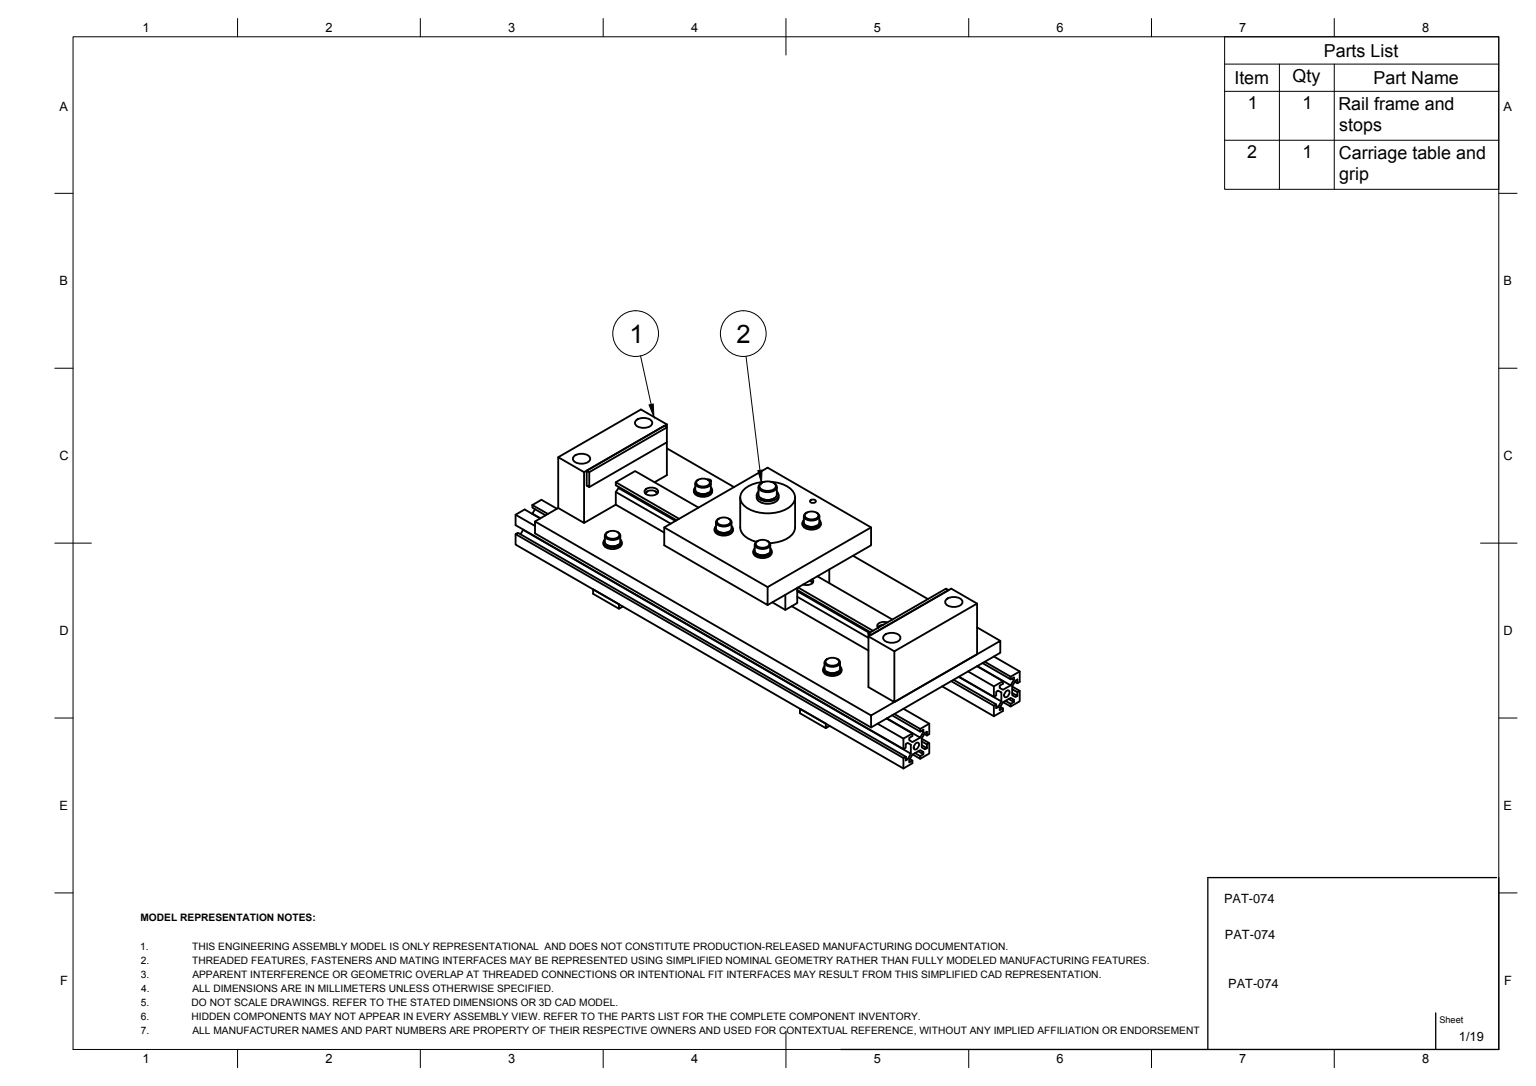
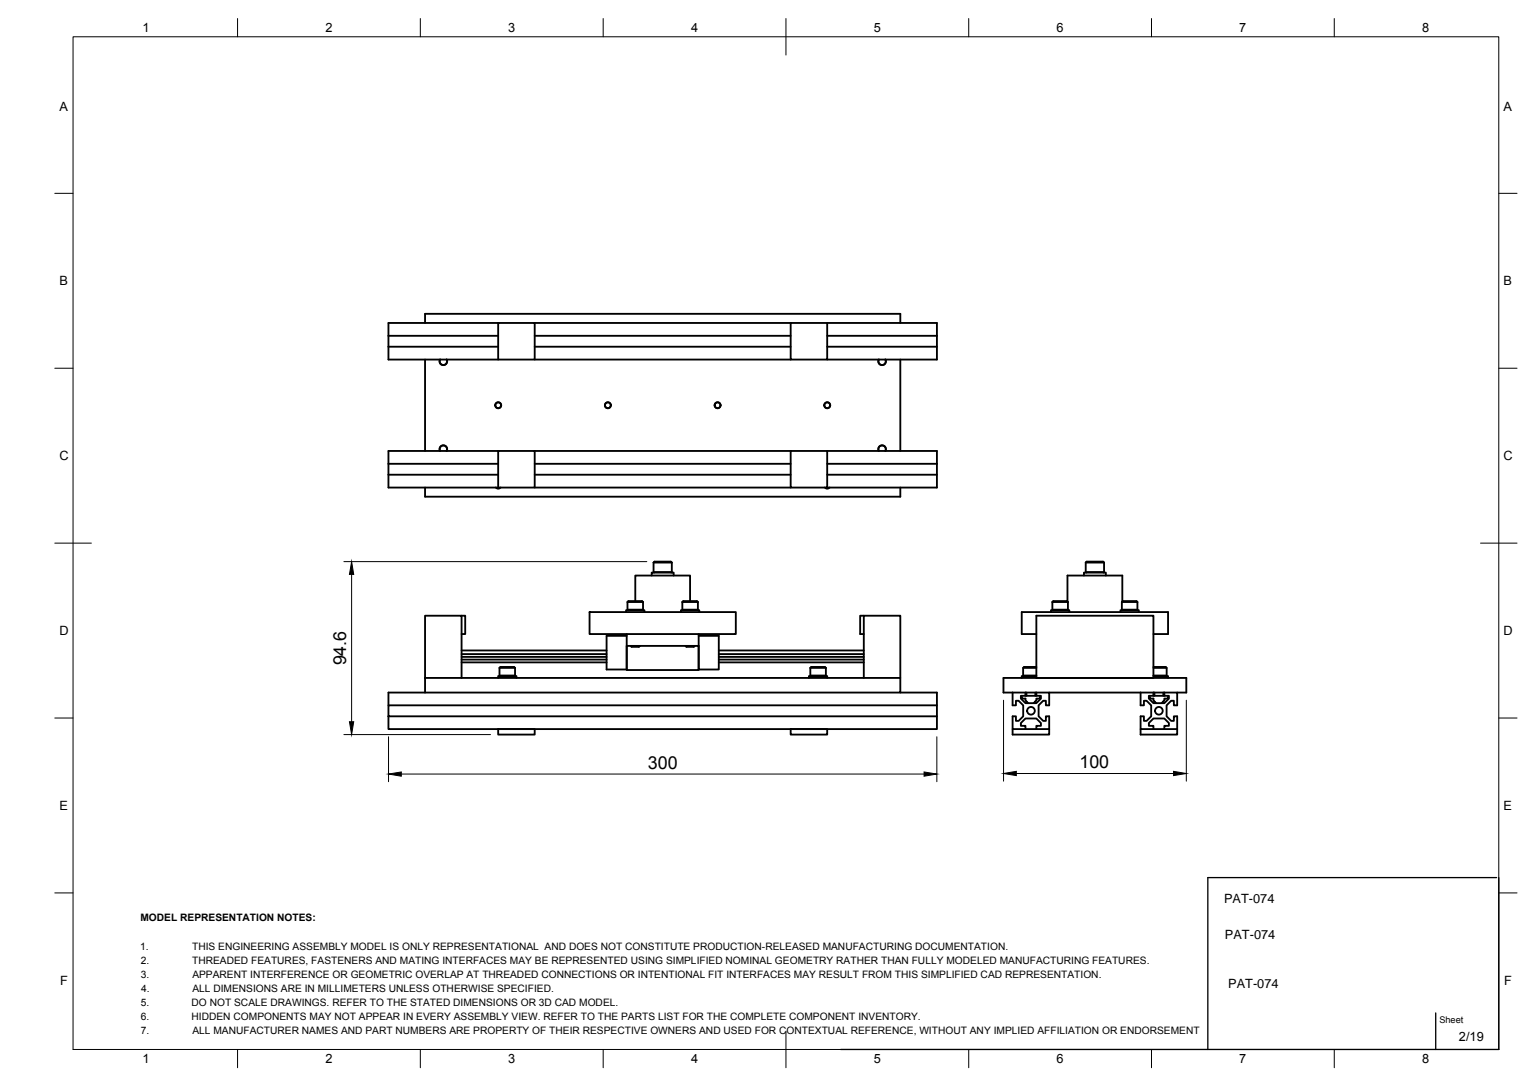
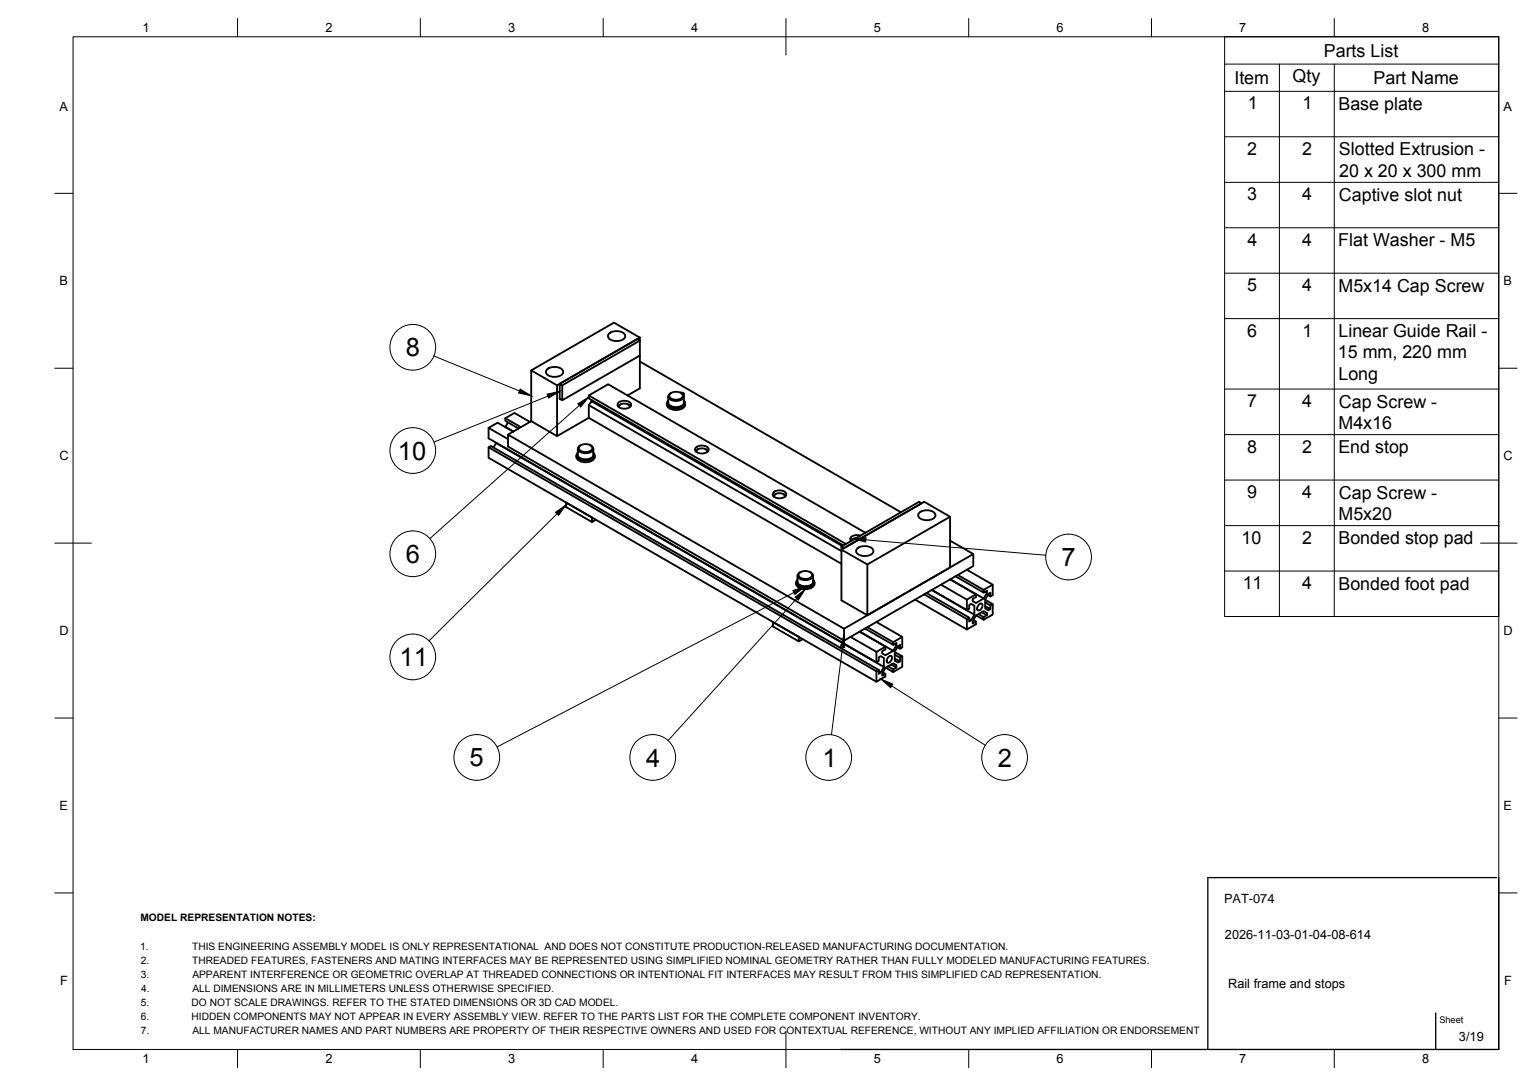
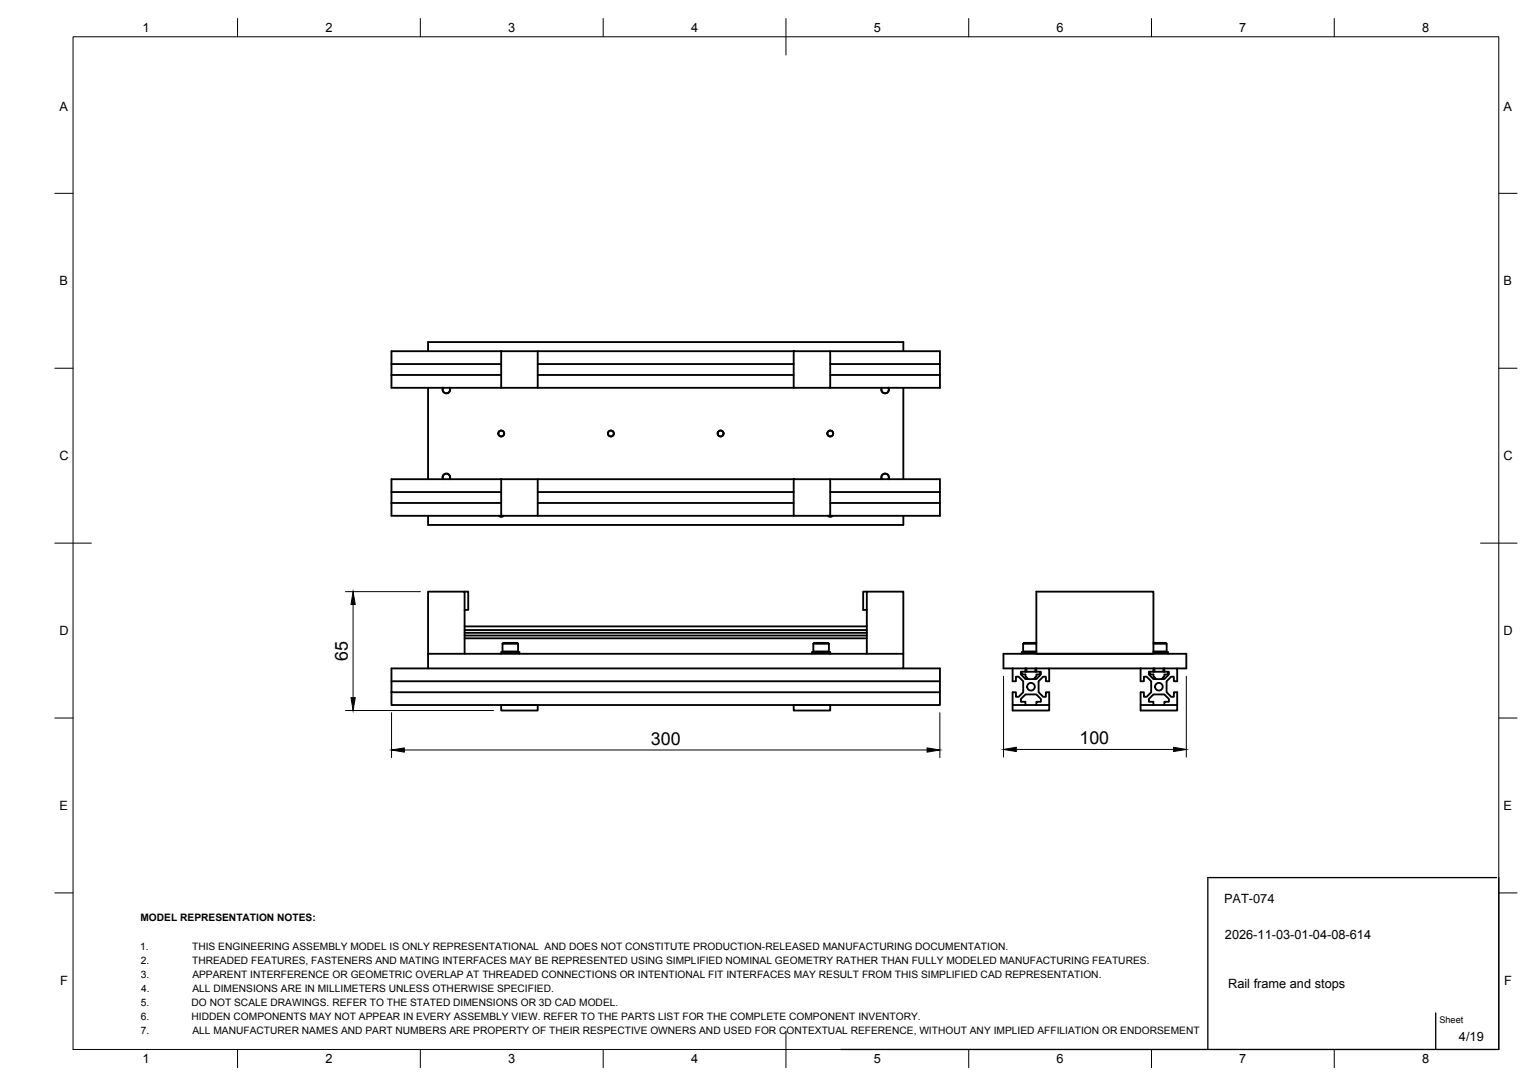
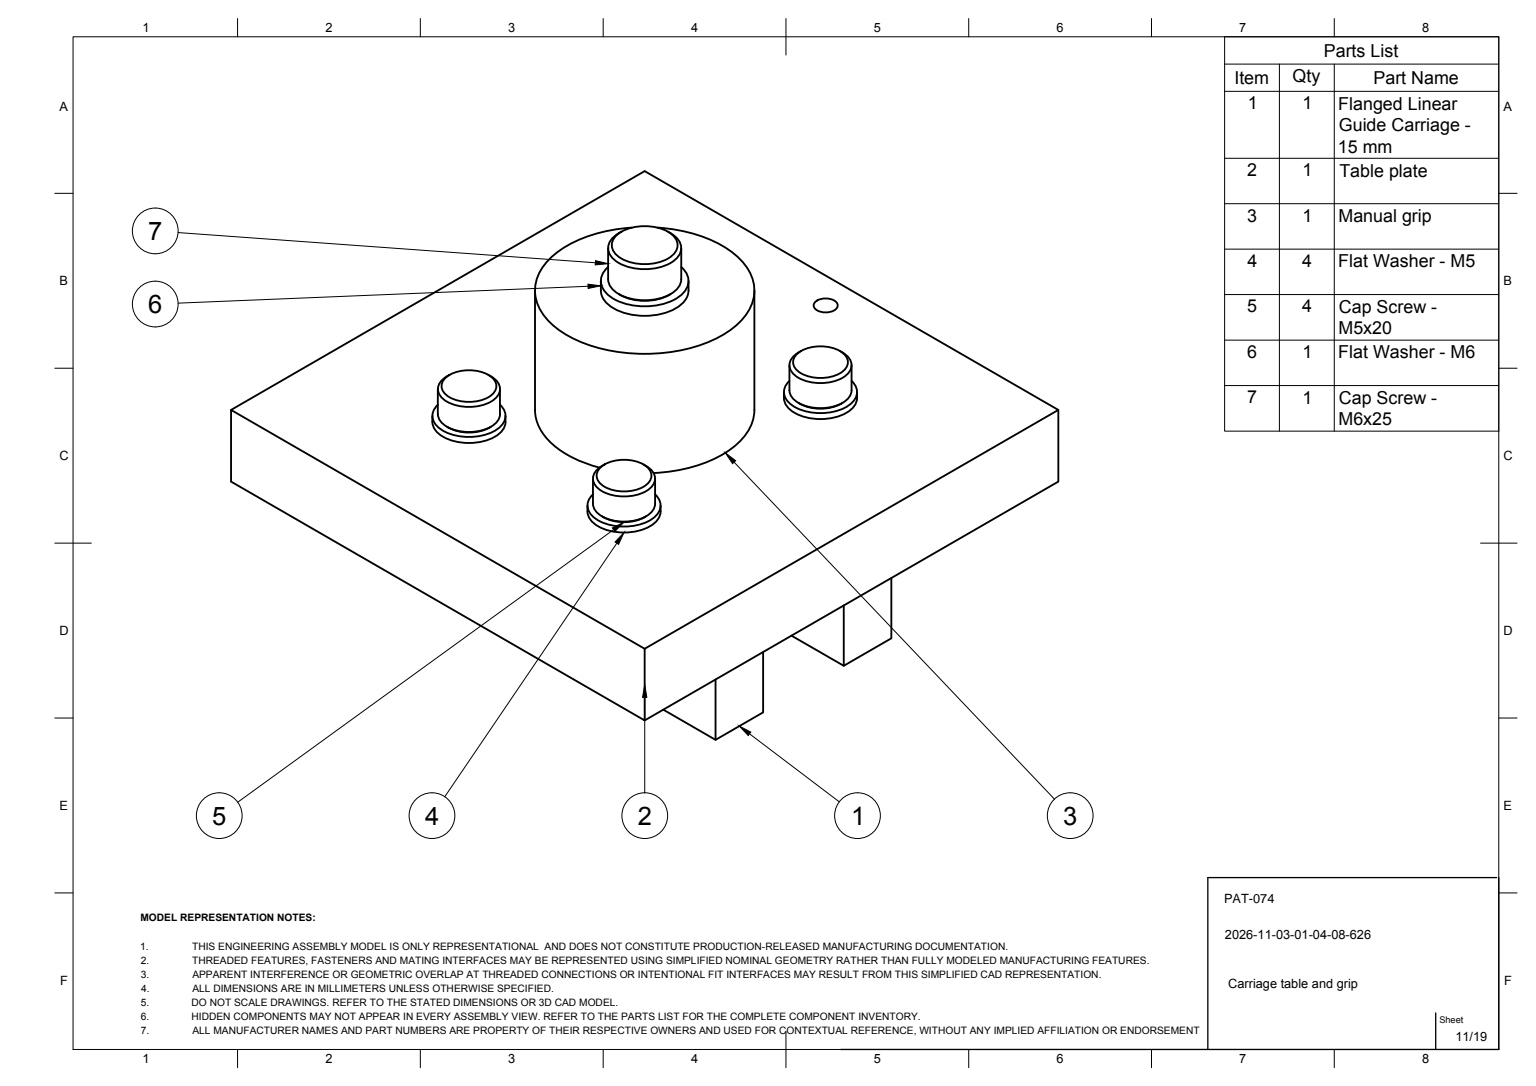
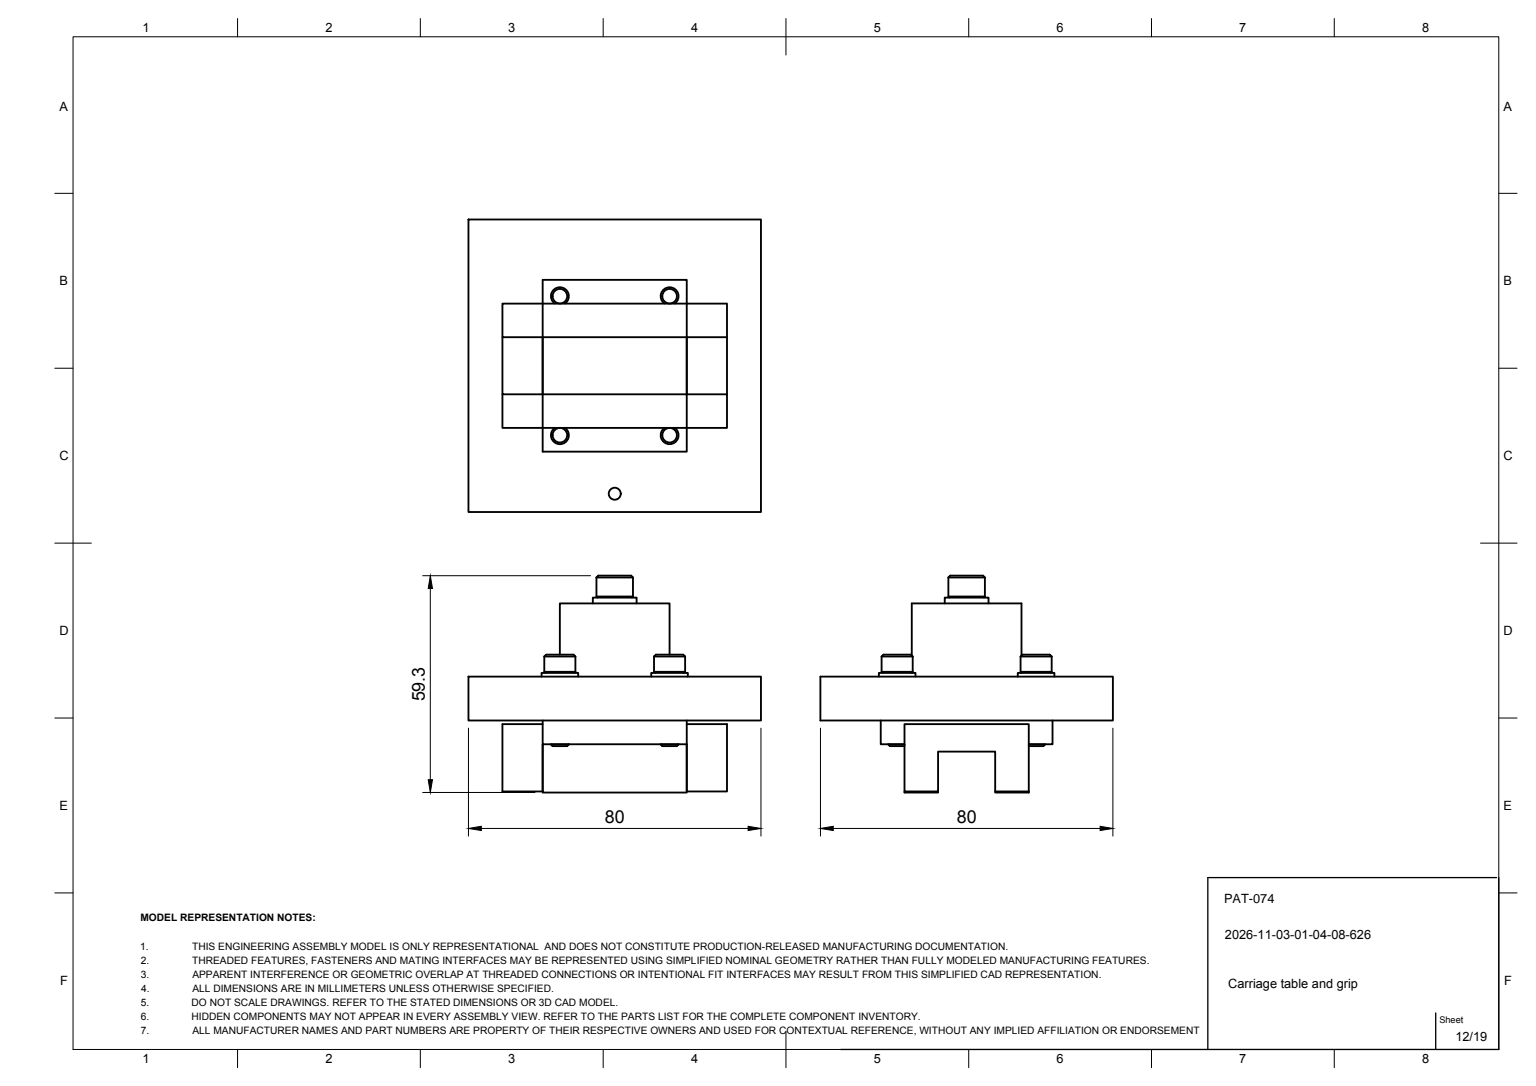
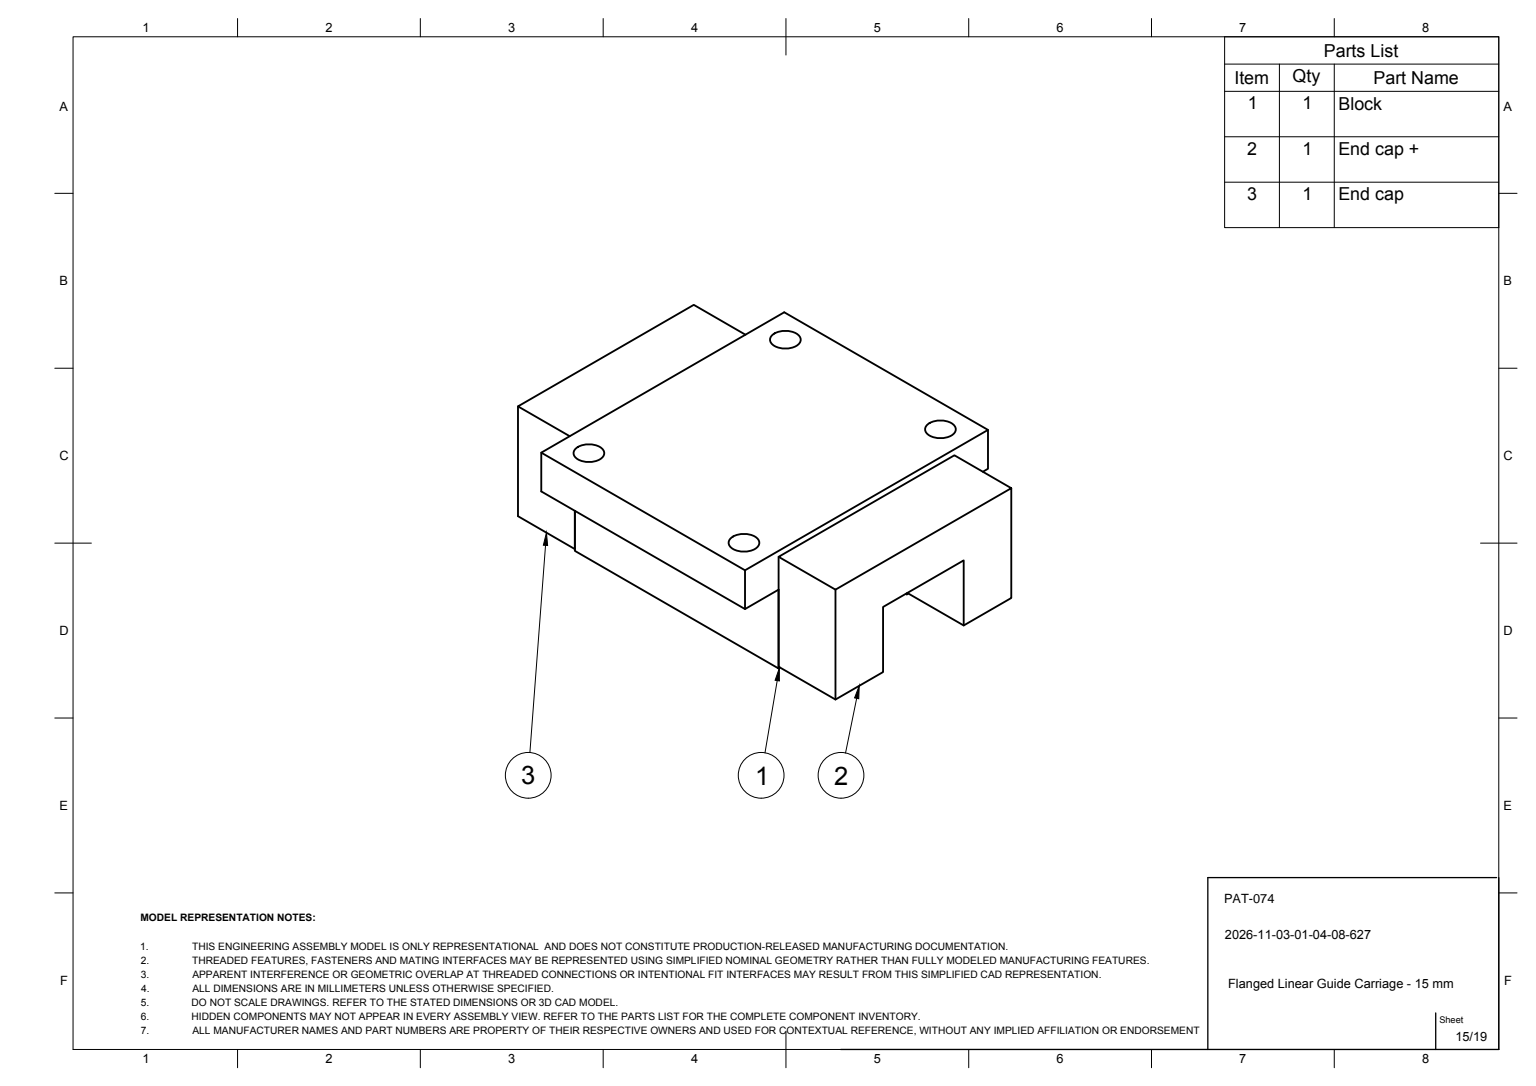
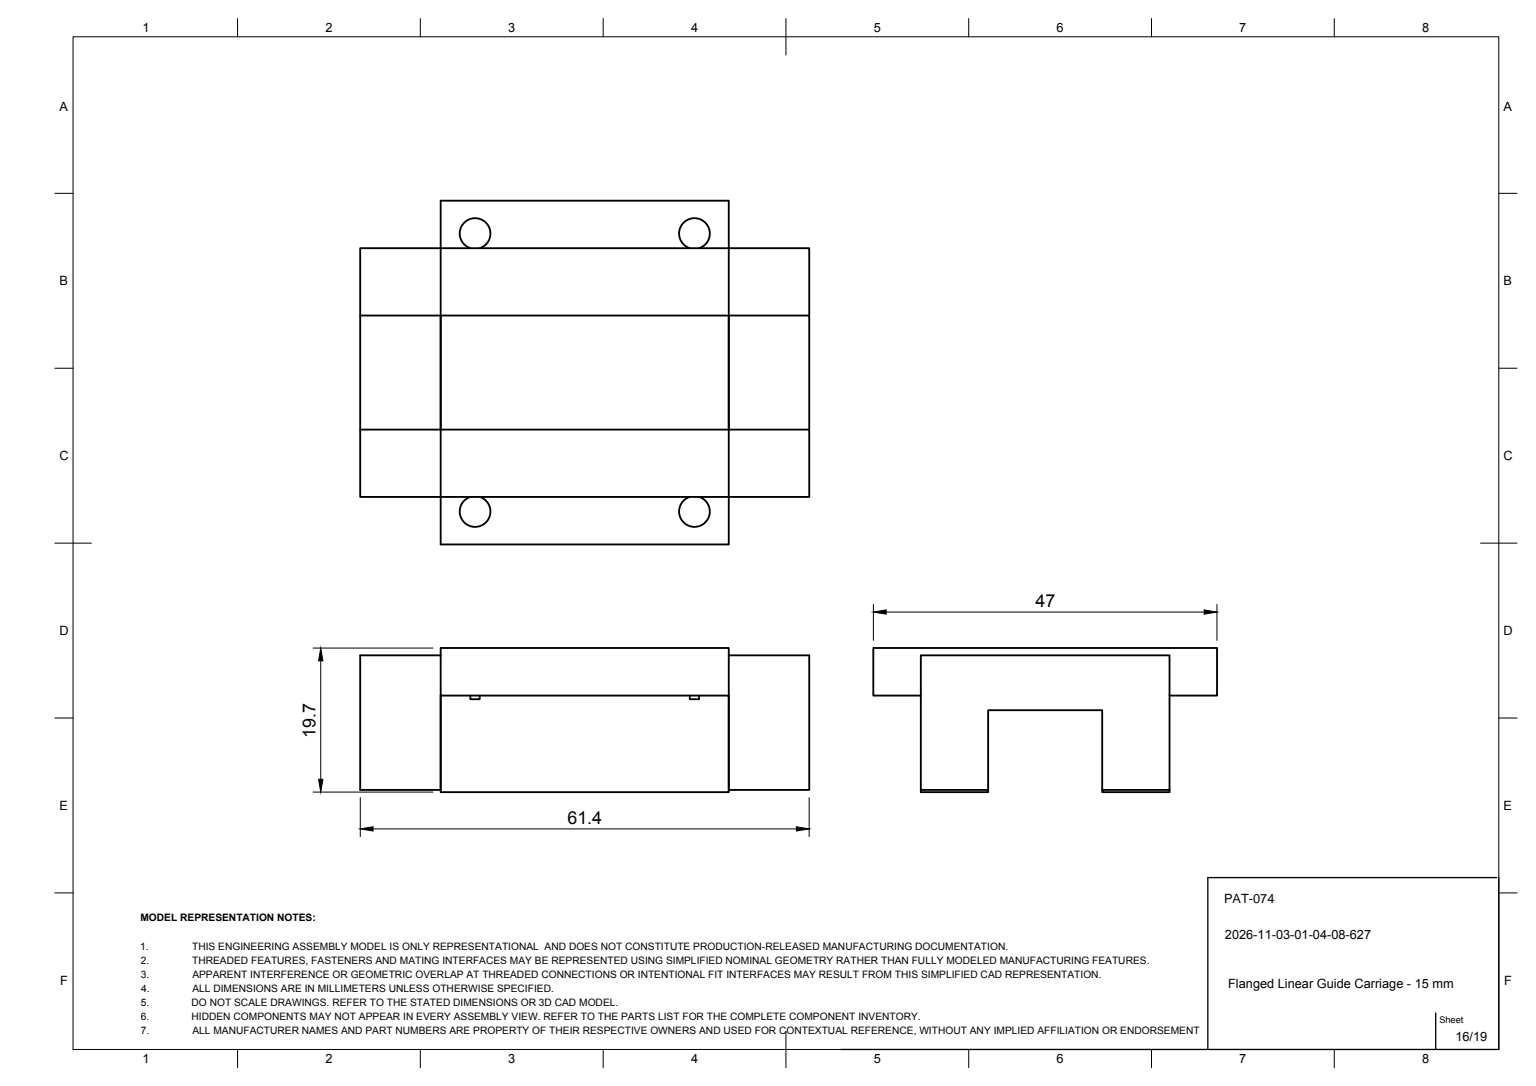
ISO-10303-21;
HEADER;
/* Generated by software containing ST-Developer
 * from STEP Tools, Inc. (www.steptools.com) 
 */

FILE_DESCRIPTION(
/* description */ ('Manual rail carriage with stops'),
/* implementation_level */ '2;1');

FILE_NAME(
/* name */ 'PAT-074',
/* time_stamp */ '2026-10-27T18:54:27-07:00',
/* author */ (''),
/* organization */ (''),
/* preprocessor_version */ 'ST-DEVELOPER v20.2',
/* originating_system */ 'Autodesk Translation Framework v15.17.0.0',
/* authorisation */ '');

FILE_SCHEMA (('AUTOMOTIVE_DESIGN { 1 0 10303 214 3 1 1 }'));
ENDSEC;

DATA;
#10=MECHANICAL_DESIGN_GEOMETRIC_PRESENTATION_REPRESENTATION('',(#273,#274,
#275,#276,#277,#278,#279,#280,#281,#282,#283,#284,#285,#286,#287,#288,#289,
#290),#8499);
#11=ITEM_DEFINED_TRANSFORMATION($,$,#5414,#5475);
#12=ITEM_DEFINED_TRANSFORMATION($,$,#5453,#5476);
#13=ITEM_DEFINED_TRANSFORMATION($,$,#5464,#5477);
#14=ITEM_DEFINED_TRANSFORMATION($,$,#5164,#5549);
#15=ITEM_DEFINED_TRANSFORMATION($,$,#5213,#5550);
#16=ITEM_DEFINED_TRANSFORMATION($,$,#5213,#5551);
#17=ITEM_DEFINED_TRANSFORMATION($,$,#5263,#5552);
#18=ITEM_DEFINED_TRANSFORMATION($,$,#5512,#5553);
#19=ITEM_DEFINED_TRANSFORMATION($,$,#5284,#5554);
#20=ITEM_DEFINED_TRANSFORMATION($,$,#5263,#5555);
#21=ITEM_DEFINED_TRANSFORMATION($,$,#5512,#5556);
#22=ITEM_DEFINED_TRANSFORMATION($,$,#5284,#5557);
#23=ITEM_DEFINED_TRANSFORMATION($,$,#5263,#5558);
#24=ITEM_DEFINED_TRANSFORMATION($,$,#5512,#5559);
#25=ITEM_DEFINED_TRANSFORMATION($,$,#5284,#5560);
#26=ITEM_DEFINED_TRANSFORMATION($,$,#5263,#5561);
#27=ITEM_DEFINED_TRANSFORMATION($,$,#5512,#5562);
#28=ITEM_DEFINED_TRANSFORMATION($,$,#5284,#5563);
#29=ITEM_DEFINED_TRANSFORMATION($,$,#5308,#5564);
#30=ITEM_DEFINED_TRANSFORMATION($,$,#5351,#5565);
#31=ITEM_DEFINED_TRANSFORMATION($,$,#5351,#5566);
#32=ITEM_DEFINED_TRANSFORMATION($,$,#5351,#5567);
#33=ITEM_DEFINED_TRANSFORMATION($,$,#5351,#5568);
#34=ITEM_DEFINED_TRANSFORMATION($,$,#5377,#5569);
#35=ITEM_DEFINED_TRANSFORMATION($,$,#5523,#5570);
#36=ITEM_DEFINED_TRANSFORMATION($,$,#5523,#5571);
#37=ITEM_DEFINED_TRANSFORMATION($,$,#5377,#5572);
#38=ITEM_DEFINED_TRANSFORMATION($,$,#5523,#5573);
#39=ITEM_DEFINED_TRANSFORMATION($,$,#5523,#5574);
#40=ITEM_DEFINED_TRANSFORMATION($,$,#5398,#5575);
#41=ITEM_DEFINED_TRANSFORMATION($,$,#5398,#5576);
#42=ITEM_DEFINED_TRANSFORMATION($,$,#5405,#5577);
#43=ITEM_DEFINED_TRANSFORMATION($,$,#5405,#5578);
#44=ITEM_DEFINED_TRANSFORMATION($,$,#5405,#5579);
#45=ITEM_DEFINED_TRANSFORMATION($,$,#5405,#5580);
#46=ITEM_DEFINED_TRANSFORMATION($,$,#5413,#5616);
#47=ITEM_DEFINED_TRANSFORMATION($,$,#5478,#5617);
#48=ITEM_DEFINED_TRANSFORMATION($,$,#5503,#5618);
#49=ITEM_DEFINED_TRANSFORMATION($,$,#5512,#5619);
#50=ITEM_DEFINED_TRANSFORMATION($,$,#5523,#5620);
#51=ITEM_DEFINED_TRANSFORMATION($,$,#5512,#5621);
#52=ITEM_DEFINED_TRANSFORMATION($,$,#5523,#5622);
#53=ITEM_DEFINED_TRANSFORMATION($,$,#5512,#5623);
#54=ITEM_DEFINED_TRANSFORMATION($,$,#5523,#5624);
#55=ITEM_DEFINED_TRANSFORMATION($,$,#5512,#5625);
#56=ITEM_DEFINED_TRANSFORMATION($,$,#5523,#5626);
#57=ITEM_DEFINED_TRANSFORMATION($,$,#5581,#5627);
#58=ITEM_DEFINED_TRANSFORMATION($,$,#5590,#5628);
#59=ITEM_DEFINED_TRANSFORMATION($,$,#5163,#5629);
#60=ITEM_DEFINED_TRANSFORMATION($,$,#5412,#5630);
#61=(
REPRESENTATION_RELATIONSHIP($,$,#8611,#8610)
REPRESENTATION_RELATIONSHIP_WITH_TRANSFORMATION(#11)
SHAPE_REPRESENTATION_RELATIONSHIP()
);
#62=(
REPRESENTATION_RELATIONSHIP($,$,#8612,#8610)
REPRESENTATION_RELATIONSHIP_WITH_TRANSFORMATION(#12)
SHAPE_REPRESENTATION_RELATIONSHIP()
);
#63=(
REPRESENTATION_RELATIONSHIP($,$,#8613,#8610)
REPRESENTATION_RELATIONSHIP_WITH_TRANSFORMATION(#13)
SHAPE_REPRESENTATION_RELATIONSHIP()
);
#64=(
REPRESENTATION_RELATIONSHIP($,$,#8600,#8599)
REPRESENTATION_RELATIONSHIP_WITH_TRANSFORMATION(#14)
SHAPE_REPRESENTATION_RELATIONSHIP()
);
#65=(
REPRESENTATION_RELATIONSHIP($,$,#8601,#8599)
REPRESENTATION_RELATIONSHIP_WITH_TRANSFORMATION(#15)
SHAPE_REPRESENTATION_RELATIONSHIP()
);
#66=(
REPRESENTATION_RELATIONSHIP($,$,#8601,#8599)
REPRESENTATION_RELATIONSHIP_WITH_TRANSFORMATION(#16)
SHAPE_REPRESENTATION_RELATIONSHIP()
);
#67=(
REPRESENTATION_RELATIONSHIP($,$,#8602,#8599)
REPRESENTATION_RELATIONSHIP_WITH_TRANSFORMATION(#17)
SHAPE_REPRESENTATION_RELATIONSHIP()
);
#68=(
REPRESENTATION_RELATIONSHIP($,$,#8616,#8599)
REPRESENTATION_RELATIONSHIP_WITH_TRANSFORMATION(#18)
SHAPE_REPRESENTATION_RELATIONSHIP()
);
#69=(
REPRESENTATION_RELATIONSHIP($,$,#8603,#8599)
REPRESENTATION_RELATIONSHIP_WITH_TRANSFORMATION(#19)
SHAPE_REPRESENTATION_RELATIONSHIP()
);
#70=(
REPRESENTATION_RELATIONSHIP($,$,#8602,#8599)
REPRESENTATION_RELATIONSHIP_WITH_TRANSFORMATION(#20)
SHAPE_REPRESENTATION_RELATIONSHIP()
);
#71=(
REPRESENTATION_RELATIONSHIP($,$,#8616,#8599)
REPRESENTATION_RELATIONSHIP_WITH_TRANSFORMATION(#21)
SHAPE_REPRESENTATION_RELATIONSHIP()
);
#72=(
REPRESENTATION_RELATIONSHIP($,$,#8603,#8599)
REPRESENTATION_RELATIONSHIP_WITH_TRANSFORMATION(#22)
SHAPE_REPRESENTATION_RELATIONSHIP()
);
#73=(
REPRESENTATION_RELATIONSHIP($,$,#8602,#8599)
REPRESENTATION_RELATIONSHIP_WITH_TRANSFORMATION(#23)
SHAPE_REPRESENTATION_RELATIONSHIP()
);
#74=(
REPRESENTATION_RELATIONSHIP($,$,#8616,#8599)
REPRESENTATION_RELATIONSHIP_WITH_TRANSFORMATION(#24)
SHAPE_REPRESENTATION_RELATIONSHIP()
);
#75=(
REPRESENTATION_RELATIONSHIP($,$,#8603,#8599)
REPRESENTATION_RELATIONSHIP_WITH_TRANSFORMATION(#25)
SHAPE_REPRESENTATION_RELATIONSHIP()
);
#76=(
REPRESENTATION_RELATIONSHIP($,$,#8602,#8599)
REPRESENTATION_RELATIONSHIP_WITH_TRANSFORMATION(#26)
SHAPE_REPRESENTATION_RELATIONSHIP()
);
#77=(
REPRESENTATION_RELATIONSHIP($,$,#8616,#8599)
REPRESENTATION_RELATIONSHIP_WITH_TRANSFORMATION(#27)
SHAPE_REPRESENTATION_RELATIONSHIP()
);
#78=(
REPRESENTATION_RELATIONSHIP($,$,#8603,#8599)
REPRESENTATION_RELATIONSHIP_WITH_TRANSFORMATION(#28)
SHAPE_REPRESENTATION_RELATIONSHIP()
);
#79=(
REPRESENTATION_RELATIONSHIP($,$,#8604,#8599)
REPRESENTATION_RELATIONSHIP_WITH_TRANSFORMATION(#29)
SHAPE_REPRESENTATION_RELATIONSHIP()
);
#80=(
REPRESENTATION_RELATIONSHIP($,$,#8605,#8599)
REPRESENTATION_RELATIONSHIP_WITH_TRANSFORMATION(#30)
SHAPE_REPRESENTATION_RELATIONSHIP()
);
#81=(
REPRESENTATION_RELATIONSHIP($,$,#8605,#8599)
REPRESENTATION_RELATIONSHIP_WITH_TRANSFORMATION(#31)
SHAPE_REPRESENTATION_RELATIONSHIP()
);
#82=(
REPRESENTATION_RELATIONSHIP($,$,#8605,#8599)
REPRESENTATION_RELATIONSHIP_WITH_TRANSFORMATION(#32)
SHAPE_REPRESENTATION_RELATIONSHIP()
);
#83=(
REPRESENTATION_RELATIONSHIP($,$,#8605,#8599)
REPRESENTATION_RELATIONSHIP_WITH_TRANSFORMATION(#33)
SHAPE_REPRESENTATION_RELATIONSHIP()
);
#84=(
REPRESENTATION_RELATIONSHIP($,$,#8606,#8599)
REPRESENTATION_RELATIONSHIP_WITH_TRANSFORMATION(#34)
SHAPE_REPRESENTATION_RELATIONSHIP()
);
#85=(
REPRESENTATION_RELATIONSHIP($,$,#8617,#8599)
REPRESENTATION_RELATIONSHIP_WITH_TRANSFORMATION(#35)
SHAPE_REPRESENTATION_RELATIONSHIP()
);
#86=(
REPRESENTATION_RELATIONSHIP($,$,#8617,#8599)
REPRESENTATION_RELATIONSHIP_WITH_TRANSFORMATION(#36)
SHAPE_REPRESENTATION_RELATIONSHIP()
);
#87=(
REPRESENTATION_RELATIONSHIP($,$,#8606,#8599)
REPRESENTATION_RELATIONSHIP_WITH_TRANSFORMATION(#37)
SHAPE_REPRESENTATION_RELATIONSHIP()
);
#88=(
REPRESENTATION_RELATIONSHIP($,$,#8617,#8599)
REPRESENTATION_RELATIONSHIP_WITH_TRANSFORMATION(#38)
SHAPE_REPRESENTATION_RELATIONSHIP()
);
#89=(
REPRESENTATION_RELATIONSHIP($,$,#8617,#8599)
REPRESENTATION_RELATIONSHIP_WITH_TRANSFORMATION(#39)
SHAPE_REPRESENTATION_RELATIONSHIP()
);
#90=(
REPRESENTATION_RELATIONSHIP($,$,#8607,#8599)
REPRESENTATION_RELATIONSHIP_WITH_TRANSFORMATION(#40)
SHAPE_REPRESENTATION_RELATIONSHIP()
);
#91=(
REPRESENTATION_RELATIONSHIP($,$,#8607,#8599)
REPRESENTATION_RELATIONSHIP_WITH_TRANSFORMATION(#41)
SHAPE_REPRESENTATION_RELATIONSHIP()
);
#92=(
REPRESENTATION_RELATIONSHIP($,$,#8608,#8599)
REPRESENTATION_RELATIONSHIP_WITH_TRANSFORMATION(#42)
SHAPE_REPRESENTATION_RELATIONSHIP()
);
#93=(
REPRESENTATION_RELATIONSHIP($,$,#8608,#8599)
REPRESENTATION_RELATIONSHIP_WITH_TRANSFORMATION(#43)
SHAPE_REPRESENTATION_RELATIONSHIP()
);
#94=(
REPRESENTATION_RELATIONSHIP($,$,#8608,#8599)
REPRESENTATION_RELATIONSHIP_WITH_TRANSFORMATION(#44)
SHAPE_REPRESENTATION_RELATIONSHIP()
);
#95=(
REPRESENTATION_RELATIONSHIP($,$,#8608,#8599)
REPRESENTATION_RELATIONSHIP_WITH_TRANSFORMATION(#45)
SHAPE_REPRESENTATION_RELATIONSHIP()
);
#96=(
REPRESENTATION_RELATIONSHIP($,$,#8610,#8609)
REPRESENTATION_RELATIONSHIP_WITH_TRANSFORMATION(#46)
SHAPE_REPRESENTATION_RELATIONSHIP()
);
#97=(
REPRESENTATION_RELATIONSHIP($,$,#8614,#8609)
REPRESENTATION_RELATIONSHIP_WITH_TRANSFORMATION(#47)
SHAPE_REPRESENTATION_RELATIONSHIP()
);
#98=(
REPRESENTATION_RELATIONSHIP($,$,#8615,#8609)
REPRESENTATION_RELATIONSHIP_WITH_TRANSFORMATION(#48)
SHAPE_REPRESENTATION_RELATIONSHIP()
);
#99=(
REPRESENTATION_RELATIONSHIP($,$,#8616,#8609)
REPRESENTATION_RELATIONSHIP_WITH_TRANSFORMATION(#49)
SHAPE_REPRESENTATION_RELATIONSHIP()
);
#100=(
REPRESENTATION_RELATIONSHIP($,$,#8617,#8609)
REPRESENTATION_RELATIONSHIP_WITH_TRANSFORMATION(#50)
SHAPE_REPRESENTATION_RELATIONSHIP()
);
#101=(
REPRESENTATION_RELATIONSHIP($,$,#8616,#8609)
REPRESENTATION_RELATIONSHIP_WITH_TRANSFORMATION(#51)
SHAPE_REPRESENTATION_RELATIONSHIP()
);
#102=(
REPRESENTATION_RELATIONSHIP($,$,#8617,#8609)
REPRESENTATION_RELATIONSHIP_WITH_TRANSFORMATION(#52)
SHAPE_REPRESENTATION_RELATIONSHIP()
);
#103=(
REPRESENTATION_RELATIONSHIP($,$,#8616,#8609)
REPRESENTATION_RELATIONSHIP_WITH_TRANSFORMATION(#53)
SHAPE_REPRESENTATION_RELATIONSHIP()
);
#104=(
REPRESENTATION_RELATIONSHIP($,$,#8617,#8609)
REPRESENTATION_RELATIONSHIP_WITH_TRANSFORMATION(#54)
SHAPE_REPRESENTATION_RELATIONSHIP()
);
#105=(
REPRESENTATION_RELATIONSHIP($,$,#8616,#8609)
REPRESENTATION_RELATIONSHIP_WITH_TRANSFORMATION(#55)
SHAPE_REPRESENTATION_RELATIONSHIP()
);
#106=(
REPRESENTATION_RELATIONSHIP($,$,#8617,#8609)
REPRESENTATION_RELATIONSHIP_WITH_TRANSFORMATION(#56)
SHAPE_REPRESENTATION_RELATIONSHIP()
);
#107=(
REPRESENTATION_RELATIONSHIP($,$,#8618,#8609)
REPRESENTATION_RELATIONSHIP_WITH_TRANSFORMATION(#57)
SHAPE_REPRESENTATION_RELATIONSHIP()
);
#108=(
REPRESENTATION_RELATIONSHIP($,$,#8619,#8609)
REPRESENTATION_RELATIONSHIP_WITH_TRANSFORMATION(#58)
SHAPE_REPRESENTATION_RELATIONSHIP()
);
#109=(
REPRESENTATION_RELATIONSHIP($,$,#8599,#8598)
REPRESENTATION_RELATIONSHIP_WITH_TRANSFORMATION(#59)
SHAPE_REPRESENTATION_RELATIONSHIP()
);
#110=(
REPRESENTATION_RELATIONSHIP($,$,#8609,#8598)
REPRESENTATION_RELATIONSHIP_WITH_TRANSFORMATION(#60)
SHAPE_REPRESENTATION_RELATIONSHIP()
);
#111=CONTEXT_DEPENDENT_SHAPE_REPRESENTATION(#61,#8542);
#112=CONTEXT_DEPENDENT_SHAPE_REPRESENTATION(#62,#8543);
#113=CONTEXT_DEPENDENT_SHAPE_REPRESENTATION(#63,#8544);
#114=CONTEXT_DEPENDENT_SHAPE_REPRESENTATION(#64,#8549);
#115=CONTEXT_DEPENDENT_SHAPE_REPRESENTATION(#65,#8550);
#116=CONTEXT_DEPENDENT_SHAPE_REPRESENTATION(#66,#8551);
#117=CONTEXT_DEPENDENT_SHAPE_REPRESENTATION(#67,#8552);
#118=CONTEXT_DEPENDENT_SHAPE_REPRESENTATION(#68,#8553);
#119=CONTEXT_DEPENDENT_SHAPE_REPRESENTATION(#69,#8554);
#120=CONTEXT_DEPENDENT_SHAPE_REPRESENTATION(#70,#8555);
#121=CONTEXT_DEPENDENT_SHAPE_REPRESENTATION(#71,#8556);
#122=CONTEXT_DEPENDENT_SHAPE_REPRESENTATION(#72,#8557);
#123=CONTEXT_DEPENDENT_SHAPE_REPRESENTATION(#73,#8558);
#124=CONTEXT_DEPENDENT_SHAPE_REPRESENTATION(#74,#8559);
#125=CONTEXT_DEPENDENT_SHAPE_REPRESENTATION(#75,#8560);
#126=CONTEXT_DEPENDENT_SHAPE_REPRESENTATION(#76,#8561);
#127=CONTEXT_DEPENDENT_SHAPE_REPRESENTATION(#77,#8562);
#128=CONTEXT_DEPENDENT_SHAPE_REPRESENTATION(#78,#8563);
#129=CONTEXT_DEPENDENT_SHAPE_REPRESENTATION(#79,#8564);
#130=CONTEXT_DEPENDENT_SHAPE_REPRESENTATION(#80,#8565);
#131=CONTEXT_DEPENDENT_SHAPE_REPRESENTATION(#81,#8566);
#132=CONTEXT_DEPENDENT_SHAPE_REPRESENTATION(#82,#8567);
#133=CONTEXT_DEPENDENT_SHAPE_REPRESENTATION(#83,#8568);
#134=CONTEXT_DEPENDENT_SHAPE_REPRESENTATION(#84,#8569);
#135=CONTEXT_DEPENDENT_SHAPE_REPRESENTATION(#85,#8570);
#136=CONTEXT_DEPENDENT_SHAPE_REPRESENTATION(#86,#8571);
#137=CONTEXT_DEPENDENT_SHAPE_REPRESENTATION(#87,#8572);
#138=CONTEXT_DEPENDENT_SHAPE_REPRESENTATION(#88,#8573);
#139=CONTEXT_DEPENDENT_SHAPE_REPRESENTATION(#89,#8574);
#140=CONTEXT_DEPENDENT_SHAPE_REPRESENTATION(#90,#8575);
#141=CONTEXT_DEPENDENT_SHAPE_REPRESENTATION(#91,#8576);
#142=CONTEXT_DEPENDENT_SHAPE_REPRESENTATION(#92,#8577);
#143=CONTEXT_DEPENDENT_SHAPE_REPRESENTATION(#93,#8578);
#144=CONTEXT_DEPENDENT_SHAPE_REPRESENTATION(#94,#8579);
#145=CONTEXT_DEPENDENT_SHAPE_REPRESENTATION(#95,#8580);
#146=CONTEXT_DEPENDENT_SHAPE_REPRESENTATION(#96,#8583);
#147=CONTEXT_DEPENDENT_SHAPE_REPRESENTATION(#97,#8584);
#148=CONTEXT_DEPENDENT_SHAPE_REPRESENTATION(#98,#8585);
#149=CONTEXT_DEPENDENT_SHAPE_REPRESENTATION(#99,#8586);
#150=CONTEXT_DEPENDENT_SHAPE_REPRESENTATION(#100,#8587);
#151=CONTEXT_DEPENDENT_SHAPE_REPRESENTATION(#101,#8588);
#152=CONTEXT_DEPENDENT_SHAPE_REPRESENTATION(#102,#8589);
#153=CONTEXT_DEPENDENT_SHAPE_REPRESENTATION(#103,#8590);
#154=CONTEXT_DEPENDENT_SHAPE_REPRESENTATION(#104,#8591);
#155=CONTEXT_DEPENDENT_SHAPE_REPRESENTATION(#105,#8592);
#156=CONTEXT_DEPENDENT_SHAPE_REPRESENTATION(#106,#8593);
#157=CONTEXT_DEPENDENT_SHAPE_REPRESENTATION(#107,#8594);
#158=CONTEXT_DEPENDENT_SHAPE_REPRESENTATION(#108,#8595);
#159=CONTEXT_DEPENDENT_SHAPE_REPRESENTATION(#109,#8596);
#160=CONTEXT_DEPENDENT_SHAPE_REPRESENTATION(#110,#8597);
#161=NEXT_ASSEMBLY_USAGE_OCCURRENCE('Block:1','Block:1','Block:1',#8633,
#8634,'Block:1');
#162=NEXT_ASSEMBLY_USAGE_OCCURRENCE('End cap +:1','End cap +:1',
'End cap +:1',#8633,#8635,'End cap +:1');
#163=NEXT_ASSEMBLY_USAGE_OCCURRENCE('End cap:1','End cap:1','End cap:1',
#8633,#8636,'End cap:1');
#164=NEXT_ASSEMBLY_USAGE_OCCURRENCE('Base plate:2','Base plate:2',
'Base plate:2',#8622,#8623,'Base plate:2');
#165=NEXT_ASSEMBLY_USAGE_OCCURRENCE(
'Slotted Extrusion - 20 x 20 x 300 mm:2',
'Slotted Extrusion - 20 x 20 x 300 mm:2',
'Slotted Extrusion - 20 x 20 x 300 mm:2',#8622,#8624,
'Slotted Extrusion - 20 x 20 x 300 mm:2');
#166=NEXT_ASSEMBLY_USAGE_OCCURRENCE(
'Slotted Extrusion - 20 x 20 x 300 mm:3',
'Slotted Extrusion - 20 x 20 x 300 mm:3',
'Slotted Extrusion - 20 x 20 x 300 mm:3',#8622,#8624,
'Slotted Extrusion - 20 x 20 x 300 mm:3');
#167=NEXT_ASSEMBLY_USAGE_OCCURRENCE('Captive slot nut:2',
'Captive slot nut:2','Captive slot nut:2',#8622,#8625,
'Captive slot nut:2');
#168=NEXT_ASSEMBLY_USAGE_OCCURRENCE('Flat Washer - M5:2',
'Flat Washer - M5:2','Flat Washer - M5:2',#8622,#8639,
'Flat Washer - M5:2');
#169=NEXT_ASSEMBLY_USAGE_OCCURRENCE('M5x14 Cap Screw:2',
'M5x14 Cap Screw:2','M5x14 Cap Screw:2',#8622,#8626,'M5x14 Cap Screw:2');
#170=NEXT_ASSEMBLY_USAGE_OCCURRENCE('Captive slot nut:3',
'Captive slot nut:3','Captive slot nut:3',#8622,#8625,
'Captive slot nut:3');
#171=NEXT_ASSEMBLY_USAGE_OCCURRENCE('Flat Washer - M5:3',
'Flat Washer - M5:3','Flat Washer - M5:3',#8622,#8639,
'Flat Washer - M5:3');
#172=NEXT_ASSEMBLY_USAGE_OCCURRENCE('M5x14 Cap Screw:3',
'M5x14 Cap Screw:3','M5x14 Cap Screw:3',#8622,#8626,'M5x14 Cap Screw:3');
#173=NEXT_ASSEMBLY_USAGE_OCCURRENCE('Captive slot nut:4',
'Captive slot nut:4','Captive slot nut:4',#8622,#8625,
'Captive slot nut:4');
#174=NEXT_ASSEMBLY_USAGE_OCCURRENCE('Flat Washer - M5:4',
'Flat Washer - M5:4','Flat Washer - M5:4',#8622,#8639,
'Flat Washer - M5:4');
#175=NEXT_ASSEMBLY_USAGE_OCCURRENCE('M5x14 Cap Screw:4',
'M5x14 Cap Screw:4','M5x14 Cap Screw:4',#8622,#8626,'M5x14 Cap Screw:4');
#176=NEXT_ASSEMBLY_USAGE_OCCURRENCE('Captive slot nut:5',
'Captive slot nut:5','Captive slot nut:5',#8622,#8625,
'Captive slot nut:5');
#177=NEXT_ASSEMBLY_USAGE_OCCURRENCE('Flat Washer - M5:5',
'Flat Washer - M5:5','Flat Washer - M5:5',#8622,#8639,
'Flat Washer - M5:5');
#178=NEXT_ASSEMBLY_USAGE_OCCURRENCE('M5x14 Cap Screw:5',
'M5x14 Cap Screw:5','M5x14 Cap Screw:5',#8622,#8626,'M5x14 Cap Screw:5');
#179=NEXT_ASSEMBLY_USAGE_OCCURRENCE(
'Linear Guide Rail - 15 mm, 220 mm Long:2',
'Linear Guide Rail - 15 mm, 220 mm Long:2',
'Linear Guide Rail - 15 mm, 220 mm Long:2',#8622,#8627,
'Linear Guide Rail - 15 mm, 220 mm Long:2');
#180=NEXT_ASSEMBLY_USAGE_OCCURRENCE('Cap Screw - M4x16:2',
'Cap Screw - M4x16:2','Cap Screw - M4x16:2',#8622,#8628,
'Cap Screw - M4x16:2');
#181=NEXT_ASSEMBLY_USAGE_OCCURRENCE('Cap Screw - M4x16:3',
'Cap Screw - M4x16:3','Cap Screw - M4x16:3',#8622,#8628,
'Cap Screw - M4x16:3');
#182=NEXT_ASSEMBLY_USAGE_OCCURRENCE('Cap Screw - M4x16:4',
'Cap Screw - M4x16:4','Cap Screw - M4x16:4',#8622,#8628,
'Cap Screw - M4x16:4');
#183=NEXT_ASSEMBLY_USAGE_OCCURRENCE('Cap Screw - M4x16:5',
'Cap Screw - M4x16:5','Cap Screw - M4x16:5',#8622,#8628,
'Cap Screw - M4x16:5');
#184=NEXT_ASSEMBLY_USAGE_OCCURRENCE('End stop:2','End stop:2',
'End stop:2',#8622,#8629,'End stop:2');
#185=NEXT_ASSEMBLY_USAGE_OCCURRENCE('Cap Screw - M5x20:6',
'Cap Screw - M5x20:6','Cap Screw - M5x20:6',#8622,#8640,
'Cap Screw - M5x20:6');
#186=NEXT_ASSEMBLY_USAGE_OCCURRENCE('Cap Screw - M5x20:7',
'Cap Screw - M5x20:7','Cap Screw - M5x20:7',#8622,#8640,
'Cap Screw - M5x20:7');
#187=NEXT_ASSEMBLY_USAGE_OCCURRENCE('End stop:3','End stop:3',
'End stop:3',#8622,#8629,'End stop:3');
#188=NEXT_ASSEMBLY_USAGE_OCCURRENCE('Cap Screw - M5x20:8',
'Cap Screw - M5x20:8','Cap Screw - M5x20:8',#8622,#8640,
'Cap Screw - M5x20:8');
#189=NEXT_ASSEMBLY_USAGE_OCCURRENCE('Cap Screw - M5x20:9',
'Cap Screw - M5x20:9','Cap Screw - M5x20:9',#8622,#8640,
'Cap Screw - M5x20:9');
#190=NEXT_ASSEMBLY_USAGE_OCCURRENCE('Bonded stop pad:2',
'Bonded stop pad:2','Bonded stop pad:2',#8622,#8630,'Bonded stop pad:2');
#191=NEXT_ASSEMBLY_USAGE_OCCURRENCE('Bonded stop pad:3',
'Bonded stop pad:3','Bonded stop pad:3',#8622,#8630,'Bonded stop pad:3');
#192=NEXT_ASSEMBLY_USAGE_OCCURRENCE('Bonded foot pad:2',
'Bonded foot pad:2','Bonded foot pad:2',#8622,#8631,'Bonded foot pad:2');
#193=NEXT_ASSEMBLY_USAGE_OCCURRENCE('Bonded foot pad:3',
'Bonded foot pad:3','Bonded foot pad:3',#8622,#8631,'Bonded foot pad:3');
#194=NEXT_ASSEMBLY_USAGE_OCCURRENCE('Bonded foot pad:4',
'Bonded foot pad:4','Bonded foot pad:4',#8622,#8631,'Bonded foot pad:4');
#195=NEXT_ASSEMBLY_USAGE_OCCURRENCE('Bonded foot pad:5',
'Bonded foot pad:5','Bonded foot pad:5',#8622,#8631,'Bonded foot pad:5');
#196=NEXT_ASSEMBLY_USAGE_OCCURRENCE(
'Flanged Linear Guide Carriage - 15 mm:2',
'Flanged Linear Guide Carriage - 15 mm:2',
'Flanged Linear Guide Carriage - 15 mm:2',#8632,#8633,
'Flanged Linear Guide Carriage - 15 mm:2');
#197=NEXT_ASSEMBLY_USAGE_OCCURRENCE('Table plate:2','Table plate:2',
'Table plate:2',#8632,#8637,'Table plate:2');
#198=NEXT_ASSEMBLY_USAGE_OCCURRENCE('Manual grip:2','Manual grip:2',
'Manual grip:2',#8632,#8638,'Manual grip:2');
#199=NEXT_ASSEMBLY_USAGE_OCCURRENCE('Flat Washer - M5:6',
'Flat Washer - M5:6','Flat Washer - M5:6',#8632,#8639,
'Flat Washer - M5:6');
#200=NEXT_ASSEMBLY_USAGE_OCCURRENCE('Cap Screw - M5x20:2',
'Cap Screw - M5x20:2','Cap Screw - M5x20:2',#8632,#8640,
'Cap Screw - M5x20:2');
#201=NEXT_ASSEMBLY_USAGE_OCCURRENCE('Flat Washer - M5:7',
'Flat Washer - M5:7','Flat Washer - M5:7',#8632,#8639,
'Flat Washer - M5:7');
#202=NEXT_ASSEMBLY_USAGE_OCCURRENCE('Cap Screw - M5x20:3',
'Cap Screw - M5x20:3','Cap Screw - M5x20:3',#8632,#8640,
'Cap Screw - M5x20:3');
#203=NEXT_ASSEMBLY_USAGE_OCCURRENCE('Flat Washer - M5:8',
'Flat Washer - M5:8','Flat Washer - M5:8',#8632,#8639,
'Flat Washer - M5:8');
#204=NEXT_ASSEMBLY_USAGE_OCCURRENCE('Cap Screw - M5x20:4',
'Cap Screw - M5x20:4','Cap Screw - M5x20:4',#8632,#8640,
'Cap Screw - M5x20:4');
#205=NEXT_ASSEMBLY_USAGE_OCCURRENCE('Flat Washer - M5:9',
'Flat Washer - M5:9','Flat Washer - M5:9',#8632,#8639,
'Flat Washer - M5:9');
#206=NEXT_ASSEMBLY_USAGE_OCCURRENCE('Cap Screw - M5x20:5',
'Cap Screw - M5x20:5','Cap Screw - M5x20:5',#8632,#8640,
'Cap Screw - M5x20:5');
#207=NEXT_ASSEMBLY_USAGE_OCCURRENCE('Flat Washer - M6:2',
'Flat Washer - M6:2','Flat Washer - M6:2',#8632,#8641,
'Flat Washer - M6:2');
#208=NEXT_ASSEMBLY_USAGE_OCCURRENCE('Cap Screw - M6x25:2',
'Cap Screw - M6x25:2','Cap Screw - M6x25:2',#8632,#8642,
'Cap Screw - M6x25:2');
#209=NEXT_ASSEMBLY_USAGE_OCCURRENCE('Rail frame and stops:1',
'Rail frame and stops:1','Rail frame and stops:1',#8621,#8622,
'Rail frame and stops:1');
#210=NEXT_ASSEMBLY_USAGE_OCCURRENCE('Carriage table and grip:1',
'Carriage table and grip:1','Carriage table and grip:1',#8621,#8632,
'Carriage table and grip:1');
#211=CONICAL_SURFACE('',#5297,0.4,0.785398163397448);
#212=CONICAL_SURFACE('',#5301,0.41,0.785398163397448);
#213=CONICAL_SURFACE('',#5305,0.26,0.463647609000806);
#214=CONICAL_SURFACE('',#5354,0.325,0.785398163397448);
#215=CONICAL_SURFACE('',#5358,0.335,0.785398163397448);
#216=CONICAL_SURFACE('',#5362,0.21,0.463647609000806);
#217=CONICAL_SURFACE('',#5366,0.18,0.785398163397448);
#218=CONICAL_SURFACE('',#5513,0.275,0.785398163397449);
#219=CONICAL_SURFACE('',#5526,0.4,0.785398163397448);
#220=CONICAL_SURFACE('',#5530,0.41,0.785398163397448);
#221=CONICAL_SURFACE('',#5534,0.26,0.463647609000806);
#222=CONICAL_SURFACE('',#5538,0.225,0.785398163397448);
#223=CONICAL_SURFACE('',#5593,0.475,0.785398163397449);
#224=CONICAL_SURFACE('',#5597,0.485,0.785398163397448);
#225=CONICAL_SURFACE('',#5601,0.31,0.463647609000806);
#226=CONICAL_SURFACE('',#5605,0.27,0.785398163397448);
#227=ORIENTED_CLOSED_SHELL('',*,#4944,.F.);
#228=ORIENTED_CLOSED_SHELL('',*,#4948,.F.);
#229=ORIENTED_CLOSED_SHELL('',*,#4959,.F.);
#230=ORIENTED_CLOSED_SHELL('',*,#4962,.F.);
#231=BREP_WITH_VOIDS('Body1',#4945,(#227));
#232=BREP_WITH_VOIDS('Body1',#4947,(#228));
#233=BREP_WITH_VOIDS('Body1',#4958,(#229));
#234=BREP_WITH_VOIDS('Body1',#4961,(#230));
#235=ELLIPSE('',#5274,0.299389011154384,0.2117);
#236=ELLIPSE('',#5278,0.299389011154384,0.2117);
#237=SHAPE_REPRESENTATION_RELATIONSHIP('SRR','None',#8600,#255);
#238=SHAPE_REPRESENTATION_RELATIONSHIP('SRR','None',#8601,#256);
#239=SHAPE_REPRESENTATION_RELATIONSHIP('SRR','None',#8602,#257);
#240=SHAPE_REPRESENTATION_RELATIONSHIP('SRR','None',#8603,#258);
#241=SHAPE_REPRESENTATION_RELATIONSHIP('SRR','None',#8604,#259);
#242=SHAPE_REPRESENTATION_RELATIONSHIP('SRR','None',#8605,#260);
#243=SHAPE_REPRESENTATION_RELATIONSHIP('SRR','None',#8606,#261);
#244=SHAPE_REPRESENTATION_RELATIONSHIP('SRR','None',#8607,#262);
#245=SHAPE_REPRESENTATION_RELATIONSHIP('SRR','None',#8608,#263);
#246=SHAPE_REPRESENTATION_RELATIONSHIP('SRR','None',#8611,#264);
#247=SHAPE_REPRESENTATION_RELATIONSHIP('SRR','None',#8612,#265);
#248=SHAPE_REPRESENTATION_RELATIONSHIP('SRR','None',#8613,#266);
#249=SHAPE_REPRESENTATION_RELATIONSHIP('SRR','None',#8614,#267);
#250=SHAPE_REPRESENTATION_RELATIONSHIP('SRR','None',#8615,#268);
#251=SHAPE_REPRESENTATION_RELATIONSHIP('SRR','None',#8616,#269);
#252=SHAPE_REPRESENTATION_RELATIONSHIP('SRR','None',#8617,#270);
#253=SHAPE_REPRESENTATION_RELATIONSHIP('SRR','None',#8618,#271);
#254=SHAPE_REPRESENTATION_RELATIONSHIP('SRR','None',#8619,#272);
#255=ADVANCED_BREP_SHAPE_REPRESENTATION('',(#291),#8479);
#256=ADVANCED_BREP_SHAPE_REPRESENTATION('',(#292),#8480);
#257=ADVANCED_BREP_SHAPE_REPRESENTATION('',(#293),#8481);
#258=ADVANCED_BREP_SHAPE_REPRESENTATION('',(#231),#8482);
#259=ADVANCED_BREP_SHAPE_REPRESENTATION('',(#294),#8483);
#260=ADVANCED_BREP_SHAPE_REPRESENTATION('',(#232),#8484);
#261=ADVANCED_BREP_SHAPE_REPRESENTATION('',(#295),#8485);
#262=ADVANCED_BREP_SHAPE_REPRESENTATION('',(#296),#8486);
#263=ADVANCED_BREP_SHAPE_REPRESENTATION('',(#297),#8487);
#264=ADVANCED_BREP_SHAPE_REPRESENTATION('',(#298),#8490);
#265=ADVANCED_BREP_SHAPE_REPRESENTATION('',(#299),#8491);
#266=ADVANCED_BREP_SHAPE_REPRESENTATION('',(#300),#8492);
#267=ADVANCED_BREP_SHAPE_REPRESENTATION('',(#301),#8493);
#268=ADVANCED_BREP_SHAPE_REPRESENTATION('',(#302),#8494);
#269=ADVANCED_BREP_SHAPE_REPRESENTATION('',(#303),#8495);
#270=ADVANCED_BREP_SHAPE_REPRESENTATION('',(#233),#8496);
#271=ADVANCED_BREP_SHAPE_REPRESENTATION('',(#304),#8497);
#272=ADVANCED_BREP_SHAPE_REPRESENTATION('',(#234),#8498);
#273=STYLED_ITEM('',(#8767),#291);
#274=STYLED_ITEM('',(#8802),#292);
#275=STYLED_ITEM('',(#8795),#293);
#276=STYLED_ITEM('',(#8795),#231);
#277=STYLED_ITEM('',(#8781),#294);
#278=STYLED_ITEM('',(#8795),#232);
#279=STYLED_ITEM('',(#8781),#295);
#280=STYLED_ITEM('',(#8802),#296);
#281=STYLED_ITEM('',(#8781),#297);
#282=STYLED_ITEM('',(#8767),#298);
#283=STYLED_ITEM('',(#8781),#299);
#284=STYLED_ITEM('',(#8802),#300);
#285=STYLED_ITEM('',(#8781),#301);
#286=STYLED_ITEM('',(#8795),#302);
#287=STYLED_ITEM('',(#8795),#303);
#288=STYLED_ITEM('',(#8795),#233);
#289=STYLED_ITEM('',(#8795),#304);
#290=STYLED_ITEM('',(#8795),#234);
#291=MANIFOLD_SOLID_BREP('Body1',#4941);
#292=MANIFOLD_SOLID_BREP('Body1',#4942);
#293=MANIFOLD_SOLID_BREP('Body1',#4943);
#294=MANIFOLD_SOLID_BREP('Body1',#4946);
#295=MANIFOLD_SOLID_BREP('Body1',#4949);
#296=MANIFOLD_SOLID_BREP('Body1',#4950);
#297=MANIFOLD_SOLID_BREP('Body1',#4951);
#298=MANIFOLD_SOLID_BREP('Body1',#4952);
#299=MANIFOLD_SOLID_BREP('Body1',#4953);
#300=MANIFOLD_SOLID_BREP('Body1',#4954);
#301=MANIFOLD_SOLID_BREP('Body1',#4955);
#302=MANIFOLD_SOLID_BREP('Body1',#4956);
#303=MANIFOLD_SOLID_BREP('Body1',#4957);
#304=MANIFOLD_SOLID_BREP('Body1',#4960);
#305=FACE_BOUND('',#861,.T.);
#306=FACE_BOUND('',#862,.T.);
#307=FACE_BOUND('',#863,.T.);
#308=FACE_BOUND('',#864,.T.);
#309=FACE_BOUND('',#865,.T.);
#310=FACE_BOUND('',#866,.T.);
#311=FACE_BOUND('',#867,.T.);
#312=FACE_BOUND('',#868,.T.);
#313=FACE_BOUND('',#869,.T.);
#314=FACE_BOUND('',#870,.T.);
#315=FACE_BOUND('',#871,.T.);
#316=FACE_BOUND('',#872,.T.);
#317=FACE_BOUND('',#873,.T.);
#318=FACE_BOUND('',#874,.T.);
#319=FACE_BOUND('',#876,.T.);
#320=FACE_BOUND('',#877,.T.);
#321=FACE_BOUND('',#878,.T.);
#322=FACE_BOUND('',#879,.T.);
#323=FACE_BOUND('',#880,.T.);
#324=FACE_BOUND('',#881,.T.);
#325=FACE_BOUND('',#882,.T.);
#326=FACE_BOUND('',#883,.T.);
#327=FACE_BOUND('',#884,.T.);
#328=FACE_BOUND('',#885,.T.);
#329=FACE_BOUND('',#886,.T.);
#330=FACE_BOUND('',#887,.T.);
#331=FACE_BOUND('',#888,.T.);
#332=FACE_BOUND('',#889,.T.);
#333=FACE_BOUND('',#936,.T.);
#334=FACE_BOUND('',#938,.T.);
#335=FACE_BOUND('',#942,.T.);
#336=FACE_BOUND('',#968,.T.);
#337=FACE_BOUND('',#973,.T.);
#338=FACE_BOUND('',#976,.T.);
#339=FACE_BOUND('',#979,.T.);
#340=FACE_BOUND('',#982,.T.);
#341=FACE_BOUND('',#992,.T.);
#342=FACE_BOUND('',#993,.T.);
#343=FACE_BOUND('',#994,.T.);
#344=FACE_BOUND('',#995,.T.);
#345=FACE_BOUND('',#1002,.T.);
#346=FACE_BOUND('',#1003,.T.);
#347=FACE_BOUND('',#1004,.T.);
#348=FACE_BOUND('',#1005,.T.);
#349=FACE_BOUND('',#1014,.T.);
#350=FACE_BOUND('',#1029,.T.);
#351=FACE_BOUND('',#1032,.T.);
#352=FACE_BOUND('',#1040,.T.);
#353=FACE_BOUND('',#1041,.T.);
#354=FACE_BOUND('',#1043,.T.);
#355=FACE_BOUND('',#1044,.T.);
#356=FACE_BOUND('',#1071,.T.);
#357=FACE_BOUND('',#1072,.T.);
#358=FACE_BOUND('',#1073,.T.);
#359=FACE_BOUND('',#1074,.T.);
#360=FACE_BOUND('',#1114,.T.);
#361=FACE_BOUND('',#1115,.T.);
#362=FACE_BOUND('',#1116,.T.);
#363=FACE_BOUND('',#1117,.T.);
#364=FACE_BOUND('',#1118,.T.);
#365=FACE_BOUND('',#1119,.T.);
#366=FACE_BOUND('',#1121,.T.);
#367=FACE_BOUND('',#1122,.T.);
#368=FACE_BOUND('',#1123,.T.);
#369=FACE_BOUND('',#1124,.T.);
#370=FACE_BOUND('',#1125,.T.);
#371=FACE_BOUND('',#1126,.T.);
#372=FACE_BOUND('',#1130,.T.);
#373=FACE_BOUND('',#1132,.T.);
#374=FACE_BOUND('',#1136,.T.);
#375=FACE_BOUND('',#1139,.T.);
#376=FACE_BOUND('',#1145,.T.);
#377=FACE_BOUND('',#1161,.T.);
#378=FACE_BOUND('',#1163,.T.);
#379=FACE_BOUND('',#1169,.T.);
#380=PLANE('',#5207);
#381=PLANE('',#5208);
#382=PLANE('',#5209);
#383=PLANE('',#5210);
#384=PLANE('',#5211);
#385=PLANE('',#5212);
#386=PLANE('',#5214);
#387=PLANE('',#5215);
#388=PLANE('',#5216);
#389=PLANE('',#5217);
#390=PLANE('',#5218);
#391=PLANE('',#5219);
#392=PLANE('',#5220);
#393=PLANE('',#5221);
#394=PLANE('',#5222);
#395=PLANE('',#5223);
#396=PLANE('',#5224);
#397=PLANE('',#5225);
#398=PLANE('',#5226);
#399=PLANE('',#5227);
#400=PLANE('',#5228);
#401=PLANE('',#5229);
#402=PLANE('',#5230);
#403=PLANE('',#5231);
#404=PLANE('',#5232);
#405=PLANE('',#5233);
#406=PLANE('',#5234);
#407=PLANE('',#5235);
#408=PLANE('',#5236);
#409=PLANE('',#5237);
#410=PLANE('',#5238);
#411=PLANE('',#5239);
#412=PLANE('',#5240);
#413=PLANE('',#5241);
#414=PLANE('',#5242);
#415=PLANE('',#5243);
#416=PLANE('',#5244);
#417=PLANE('',#5245);
#418=PLANE('',#5246);
#419=PLANE('',#5247);
#420=PLANE('',#5248);
#421=PLANE('',#5249);
#422=PLANE('',#5253);
#423=PLANE('',#5254);
#424=PLANE('',#5255);
#425=PLANE('',#5256);
#426=PLANE('',#5257);
#427=PLANE('',#5258);
#428=PLANE('',#5259);
#429=PLANE('',#5260);
#430=PLANE('',#5261);
#431=PLANE('',#5262);
#432=PLANE('',#5264);
#433=PLANE('',#5265);
#434=PLANE('',#5266);
#435=PLANE('',#5268);
#436=PLANE('',#5269);
#437=PLANE('',#5270);
#438=PLANE('',#5271);
#439=PLANE('',#5272);
#440=PLANE('',#5273);
#441=PLANE('',#5280);
#442=PLANE('',#5281);
#443=PLANE('',#5282);
#444=PLANE('',#5283);
#445=PLANE('',#5285);
#446=PLANE('',#5286);
#447=PLANE('',#5287);
#448=PLANE('',#5288);
#449=PLANE('',#5289);
#450=PLANE('',#5290);
#451=PLANE('',#5291);
#452=PLANE('',#5292);
#453=PLANE('',#5293);
#454=PLANE('',#5295);
#455=PLANE('',#5303);
#456=PLANE('',#5312);
#457=PLANE('',#5317);
#458=PLANE('',#5322);
#459=PLANE('',#5327);
#460=PLANE('',#5337);
#461=PLANE('',#5338);
#462=PLANE('',#5339);
#463=PLANE('',#5340);
#464=PLANE('',#5341);
#465=PLANE('',#5342);
#466=PLANE('',#5343);
#467=PLANE('',#5344);
#468=PLANE('',#5345);
#469=PLANE('',#5346);
#470=PLANE('',#5347);
#471=PLANE('',#5348);
#472=PLANE('',#5349);
#473=PLANE('',#5350);
#474=PLANE('',#5352);
#475=PLANE('',#5360);
#476=PLANE('',#5368);
#477=PLANE('',#5369);
#478=PLANE('',#5370);
#479=PLANE('',#5371);
#480=PLANE('',#5372);
#481=PLANE('',#5373);
#482=PLANE('',#5374);
#483=PLANE('',#5375);
#484=PLANE('',#5376);
#485=PLANE('',#5381);
#486=PLANE('',#5386);
#487=PLANE('',#5392);
#488=PLANE('',#5393);
#489=PLANE('',#5394);
#490=PLANE('',#5395);
#491=PLANE('',#5396);
#492=PLANE('',#5397);
#493=PLANE('',#5399);
#494=PLANE('',#5400);
#495=PLANE('',#5401);
#496=PLANE('',#5402);
#497=PLANE('',#5403);
#498=PLANE('',#5404);
#499=PLANE('',#5406);
#500=PLANE('',#5407);
#501=PLANE('',#5408);
#502=PLANE('',#5409);
#503=PLANE('',#5410);
#504=PLANE('',#5411);
#505=PLANE('',#5415);
#506=PLANE('',#5421);
#507=PLANE('',#5427);
#508=PLANE('',#5433);
#509=PLANE('',#5439);
#510=PLANE('',#5440);
#511=PLANE('',#5441);
#512=PLANE('',#5442);
#513=PLANE('',#5443);
#514=PLANE('',#5444);
#515=PLANE('',#5445);
#516=PLANE('',#5446);
#517=PLANE('',#5447);
#518=PLANE('',#5448);
#519=PLANE('',#5449);
#520=PLANE('',#5450);
#521=PLANE('',#5451);
#522=PLANE('',#5452);
#523=PLANE('',#5454);
#524=PLANE('',#5455);
#525=PLANE('',#5456);
#526=PLANE('',#5457);
#527=PLANE('',#5458);
#528=PLANE('',#5459);
#529=PLANE('',#5460);
#530=PLANE('',#5461);
#531=PLANE('',#5462);
#532=PLANE('',#5463);
#533=PLANE('',#5465);
#534=PLANE('',#5466);
#535=PLANE('',#5467);
#536=PLANE('',#5468);
#537=PLANE('',#5469);
#538=PLANE('',#5470);
#539=PLANE('',#5471);
#540=PLANE('',#5472);
#541=PLANE('',#5473);
#542=PLANE('',#5474);
#543=PLANE('',#5497);
#544=PLANE('',#5498);
#545=PLANE('',#5499);
#546=PLANE('',#5500);
#547=PLANE('',#5501);
#548=PLANE('',#5502);
#549=PLANE('',#5510);
#550=PLANE('',#5511);
#551=PLANE('',#5518);
#552=PLANE('',#5522);
#553=PLANE('',#5524);
#554=PLANE('',#5532);
#555=PLANE('',#5540);
#556=PLANE('',#5541);
#557=PLANE('',#5542);
#558=PLANE('',#5543);
#559=PLANE('',#5544);
#560=PLANE('',#5545);
#561=PLANE('',#5546);
#562=PLANE('',#5547);
#563=PLANE('',#5548);
#564=PLANE('',#5588);
#565=PLANE('',#5589);
#566=PLANE('',#5591);
#567=PLANE('',#5599);
#568=PLANE('',#5607);
#569=PLANE('',#5608);
#570=PLANE('',#5609);
#571=PLANE('',#5610);
#572=PLANE('',#5611);
#573=PLANE('',#5612);
#574=PLANE('',#5613);
#575=PLANE('',#5614);
#576=PLANE('',#5615);
#577=FACE_OUTER_BOUND('',#842,.T.);
#578=FACE_OUTER_BOUND('',#843,.T.);
#579=FACE_OUTER_BOUND('',#844,.T.);
#580=FACE_OUTER_BOUND('',#845,.T.);
#581=FACE_OUTER_BOUND('',#846,.T.);
#582=FACE_OUTER_BOUND('',#847,.T.);
#583=FACE_OUTER_BOUND('',#848,.T.);
#584=FACE_OUTER_BOUND('',#849,.T.);
#585=FACE_OUTER_BOUND('',#850,.T.);
#586=FACE_OUTER_BOUND('',#851,.T.);
#587=FACE_OUTER_BOUND('',#852,.T.);
#588=FACE_OUTER_BOUND('',#853,.T.);
#589=FACE_OUTER_BOUND('',#854,.T.);
#590=FACE_OUTER_BOUND('',#855,.T.);
#591=FACE_OUTER_BOUND('',#856,.T.);
#592=FACE_OUTER_BOUND('',#857,.T.);
#593=FACE_OUTER_BOUND('',#858,.T.);
#594=FACE_OUTER_BOUND('',#859,.T.);
#595=FACE_OUTER_BOUND('',#860,.T.);
#596=FACE_OUTER_BOUND('',#875,.T.);
#597=FACE_OUTER_BOUND('',#890,.T.);
#598=FACE_OUTER_BOUND('',#891,.T.);
#599=FACE_OUTER_BOUND('',#892,.T.);
#600=FACE_OUTER_BOUND('',#893,.T.);
#601=FACE_OUTER_BOUND('',#894,.T.);
#602=FACE_OUTER_BOUND('',#895,.T.);
#603=FACE_OUTER_BOUND('',#896,.T.);
#604=FACE_OUTER_BOUND('',#897,.T.);
#605=FACE_OUTER_BOUND('',#898,.T.);
#606=FACE_OUTER_BOUND('',#899,.T.);
#607=FACE_OUTER_BOUND('',#900,.T.);
#608=FACE_OUTER_BOUND('',#901,.T.);
#609=FACE_OUTER_BOUND('',#902,.T.);
#610=FACE_OUTER_BOUND('',#903,.T.);
#611=FACE_OUTER_BOUND('',#904,.T.);
#612=FACE_OUTER_BOUND('',#905,.T.);
#613=FACE_OUTER_BOUND('',#906,.T.);
#614=FACE_OUTER_BOUND('',#907,.T.);
#615=FACE_OUTER_BOUND('',#908,.T.);
#616=FACE_OUTER_BOUND('',#909,.T.);
#617=FACE_OUTER_BOUND('',#910,.T.);
#618=FACE_OUTER_BOUND('',#911,.T.);
#619=FACE_OUTER_BOUND('',#912,.T.);
#620=FACE_OUTER_BOUND('',#913,.T.);
#621=FACE_OUTER_BOUND('',#914,.T.);
#622=FACE_OUTER_BOUND('',#915,.T.);
#623=FACE_OUTER_BOUND('',#916,.T.);
#624=FACE_OUTER_BOUND('',#917,.T.);
#625=FACE_OUTER_BOUND('',#918,.T.);
#626=FACE_OUTER_BOUND('',#919,.T.);
#627=FACE_OUTER_BOUND('',#920,.T.);
#628=FACE_OUTER_BOUND('',#921,.T.);
#629=FACE_OUTER_BOUND('',#922,.T.);
#630=FACE_OUTER_BOUND('',#923,.T.);
#631=FACE_OUTER_BOUND('',#924,.T.);
#632=FACE_OUTER_BOUND('',#925,.T.);
#633=FACE_OUTER_BOUND('',#926,.T.);
#634=FACE_OUTER_BOUND('',#927,.T.);
#635=FACE_OUTER_BOUND('',#928,.T.);
#636=FACE_OUTER_BOUND('',#929,.T.);
#637=FACE_OUTER_BOUND('',#930,.T.);
#638=FACE_OUTER_BOUND('',#931,.T.);
#639=FACE_OUTER_BOUND('',#932,.T.);
#640=FACE_OUTER_BOUND('',#933,.T.);
#641=FACE_OUTER_BOUND('',#934,.T.);
#642=FACE_OUTER_BOUND('',#935,.T.);
#643=FACE_OUTER_BOUND('',#937,.T.);
#644=FACE_OUTER_BOUND('',#939,.T.);
#645=FACE_OUTER_BOUND('',#940,.T.);
#646=FACE_OUTER_BOUND('',#941,.T.);
#647=FACE_OUTER_BOUND('',#943,.T.);
#648=FACE_OUTER_BOUND('',#944,.T.);
#649=FACE_OUTER_BOUND('',#945,.T.);
#650=FACE_OUTER_BOUND('',#946,.T.);
#651=FACE_OUTER_BOUND('',#947,.T.);
#652=FACE_OUTER_BOUND('',#948,.T.);
#653=FACE_OUTER_BOUND('',#949,.T.);
#654=FACE_OUTER_BOUND('',#950,.T.);
#655=FACE_OUTER_BOUND('',#951,.T.);
#656=FACE_OUTER_BOUND('',#952,.T.);
#657=FACE_OUTER_BOUND('',#953,.T.);
#658=FACE_OUTER_BOUND('',#954,.T.);
#659=FACE_OUTER_BOUND('',#955,.T.);
#660=FACE_OUTER_BOUND('',#956,.T.);
#661=FACE_OUTER_BOUND('',#957,.T.);
#662=FACE_OUTER_BOUND('',#958,.T.);
#663=FACE_OUTER_BOUND('',#959,.T.);
#664=FACE_OUTER_BOUND('',#960,.T.);
#665=FACE_OUTER_BOUND('',#961,.T.);
#666=FACE_OUTER_BOUND('',#962,.T.);
#667=FACE_OUTER_BOUND('',#963,.T.);
#668=FACE_OUTER_BOUND('',#964,.T.);
#669=FACE_OUTER_BOUND('',#965,.T.);
#670=FACE_OUTER_BOUND('',#966,.T.);
#671=FACE_OUTER_BOUND('',#967,.T.);
#672=FACE_OUTER_BOUND('',#969,.T.);
#673=FACE_OUTER_BOUND('',#970,.T.);
#674=FACE_OUTER_BOUND('',#971,.T.);
#675=FACE_OUTER_BOUND('',#972,.T.);
#676=FACE_OUTER_BOUND('',#974,.T.);
#677=FACE_OUTER_BOUND('',#975,.T.);
#678=FACE_OUTER_BOUND('',#977,.T.);
#679=FACE_OUTER_BOUND('',#978,.T.);
#680=FACE_OUTER_BOUND('',#980,.T.);
#681=FACE_OUTER_BOUND('',#981,.T.);
#682=FACE_OUTER_BOUND('',#983,.T.);
#683=FACE_OUTER_BOUND('',#984,.T.);
#684=FACE_OUTER_BOUND('',#985,.T.);
#685=FACE_OUTER_BOUND('',#986,.T.);
#686=FACE_OUTER_BOUND('',#987,.T.);
#687=FACE_OUTER_BOUND('',#988,.T.);
#688=FACE_OUTER_BOUND('',#989,.T.);
#689=FACE_OUTER_BOUND('',#990,.T.);
#690=FACE_OUTER_BOUND('',#991,.T.);
#691=FACE_OUTER_BOUND('',#996,.T.);
#692=FACE_OUTER_BOUND('',#997,.T.);
#693=FACE_OUTER_BOUND('',#998,.T.);
#694=FACE_OUTER_BOUND('',#999,.T.);
#695=FACE_OUTER_BOUND('',#1000,.T.);
#696=FACE_OUTER_BOUND('',#1001,.T.);
#697=FACE_OUTER_BOUND('',#1006,.T.);
#698=FACE_OUTER_BOUND('',#1007,.T.);
#699=FACE_OUTER_BOUND('',#1008,.T.);
#700=FACE_OUTER_BOUND('',#1009,.T.);
#701=FACE_OUTER_BOUND('',#1010,.T.);
#702=FACE_OUTER_BOUND('',#1011,.T.);
#703=FACE_OUTER_BOUND('',#1012,.T.);
#704=FACE_OUTER_BOUND('',#1013,.T.);
#705=FACE_OUTER_BOUND('',#1015,.T.);
#706=FACE_OUTER_BOUND('',#1016,.T.);
#707=FACE_OUTER_BOUND('',#1017,.T.);
#708=FACE_OUTER_BOUND('',#1018,.T.);
#709=FACE_OUTER_BOUND('',#1019,.T.);
#710=FACE_OUTER_BOUND('',#1020,.T.);
#711=FACE_OUTER_BOUND('',#1021,.T.);
#712=FACE_OUTER_BOUND('',#1022,.T.);
#713=FACE_OUTER_BOUND('',#1023,.T.);
#714=FACE_OUTER_BOUND('',#1024,.T.);
#715=FACE_OUTER_BOUND('',#1025,.T.);
#716=FACE_OUTER_BOUND('',#1026,.T.);
#717=FACE_OUTER_BOUND('',#1027,.T.);
#718=FACE_OUTER_BOUND('',#1028,.T.);
#719=FACE_OUTER_BOUND('',#1030,.T.);
#720=FACE_OUTER_BOUND('',#1031,.T.);
#721=FACE_OUTER_BOUND('',#1033,.T.);
#722=FACE_OUTER_BOUND('',#1034,.T.);
#723=FACE_OUTER_BOUND('',#1035,.T.);
#724=FACE_OUTER_BOUND('',#1036,.T.);
#725=FACE_OUTER_BOUND('',#1037,.T.);
#726=FACE_OUTER_BOUND('',#1038,.T.);
#727=FACE_OUTER_BOUND('',#1039,.T.);
#728=FACE_OUTER_BOUND('',#1042,.T.);
#729=FACE_OUTER_BOUND('',#1045,.T.);
#730=FACE_OUTER_BOUND('',#1046,.T.);
#731=FACE_OUTER_BOUND('',#1047,.T.);
#732=FACE_OUTER_BOUND('',#1048,.T.);
#733=FACE_OUTER_BOUND('',#1049,.T.);
#734=FACE_OUTER_BOUND('',#1050,.T.);
#735=FACE_OUTER_BOUND('',#1051,.T.);
#736=FACE_OUTER_BOUND('',#1052,.T.);
#737=FACE_OUTER_BOUND('',#1053,.T.);
#738=FACE_OUTER_BOUND('',#1054,.T.);
#739=FACE_OUTER_BOUND('',#1055,.T.);
#740=FACE_OUTER_BOUND('',#1056,.T.);
#741=FACE_OUTER_BOUND('',#1057,.T.);
#742=FACE_OUTER_BOUND('',#1058,.T.);
#743=FACE_OUTER_BOUND('',#1059,.T.);
#744=FACE_OUTER_BOUND('',#1060,.T.);
#745=FACE_OUTER_BOUND('',#1061,.T.);
#746=FACE_OUTER_BOUND('',#1062,.T.);
#747=FACE_OUTER_BOUND('',#1063,.T.);
#748=FACE_OUTER_BOUND('',#1064,.T.);
#749=FACE_OUTER_BOUND('',#1065,.T.);
#750=FACE_OUTER_BOUND('',#1066,.T.);
#751=FACE_OUTER_BOUND('',#1067,.T.);
#752=FACE_OUTER_BOUND('',#1068,.T.);
#753=FACE_OUTER_BOUND('',#1069,.T.);
#754=FACE_OUTER_BOUND('',#1070,.T.);
#755=FACE_OUTER_BOUND('',#1075,.T.);
#756=FACE_OUTER_BOUND('',#1076,.T.);
#757=FACE_OUTER_BOUND('',#1077,.T.);
#758=FACE_OUTER_BOUND('',#1078,.T.);
#759=FACE_OUTER_BOUND('',#1079,.T.);
#760=FACE_OUTER_BOUND('',#1080,.T.);
#761=FACE_OUTER_BOUND('',#1081,.T.);
#762=FACE_OUTER_BOUND('',#1082,.T.);
#763=FACE_OUTER_BOUND('',#1083,.T.);
#764=FACE_OUTER_BOUND('',#1084,.T.);
#765=FACE_OUTER_BOUND('',#1085,.T.);
#766=FACE_OUTER_BOUND('',#1086,.T.);
#767=FACE_OUTER_BOUND('',#1087,.T.);
#768=FACE_OUTER_BOUND('',#1088,.T.);
#769=FACE_OUTER_BOUND('',#1089,.T.);
#770=FACE_OUTER_BOUND('',#1090,.T.);
#771=FACE_OUTER_BOUND('',#1091,.T.);
#772=FACE_OUTER_BOUND('',#1092,.T.);
#773=FACE_OUTER_BOUND('',#1093,.T.);
#774=FACE_OUTER_BOUND('',#1094,.T.);
#775=FACE_OUTER_BOUND('',#1095,.T.);
#776=FACE_OUTER_BOUND('',#1096,.T.);
#777=FACE_OUTER_BOUND('',#1097,.T.);
#778=FACE_OUTER_BOUND('',#1098,.T.);
#779=FACE_OUTER_BOUND('',#1099,.T.);
#780=FACE_OUTER_BOUND('',#1100,.T.);
#781=FACE_OUTER_BOUND('',#1101,.T.);
#782=FACE_OUTER_BOUND('',#1102,.T.);
#783=FACE_OUTER_BOUND('',#1103,.T.);
#784=FACE_OUTER_BOUND('',#1104,.T.);
#785=FACE_OUTER_BOUND('',#1105,.T.);
#786=FACE_OUTER_BOUND('',#1106,.T.);
#787=FACE_OUTER_BOUND('',#1107,.T.);
#788=FACE_OUTER_BOUND('',#1108,.T.);
#789=FACE_OUTER_BOUND('',#1109,.T.);
#790=FACE_OUTER_BOUND('',#1110,.T.);
#791=FACE_OUTER_BOUND('',#1111,.T.);
#792=FACE_OUTER_BOUND('',#1112,.T.);
#793=FACE_OUTER_BOUND('',#1113,.T.);
#794=FACE_OUTER_BOUND('',#1120,.T.);
#795=FACE_OUTER_BOUND('',#1127,.T.);
#796=FACE_OUTER_BOUND('',#1128,.T.);
#797=FACE_OUTER_BOUND('',#1129,.T.);
#798=FACE_OUTER_BOUND('',#1131,.T.);
#799=FACE_OUTER_BOUND('',#1133,.T.);
#800=FACE_OUTER_BOUND('',#1134,.T.);
#801=FACE_OUTER_BOUND('',#1135,.T.);
#802=FACE_OUTER_BOUND('',#1137,.T.);
#803=FACE_OUTER_BOUND('',#1138,.T.);
#804=FACE_OUTER_BOUND('',#1140,.T.);
#805=FACE_OUTER_BOUND('',#1141,.T.);
#806=FACE_OUTER_BOUND('',#1142,.T.);
#807=FACE_OUTER_BOUND('',#1143,.T.);
#808=FACE_OUTER_BOUND('',#1144,.T.);
#809=FACE_OUTER_BOUND('',#1146,.T.);
#810=FACE_OUTER_BOUND('',#1147,.T.);
#811=FACE_OUTER_BOUND('',#1148,.T.);
#812=FACE_OUTER_BOUND('',#1149,.T.);
#813=FACE_OUTER_BOUND('',#1150,.T.);
#814=FACE_OUTER_BOUND('',#1151,.T.);
#815=FACE_OUTER_BOUND('',#1152,.T.);
#816=FACE_OUTER_BOUND('',#1153,.T.);
#817=FACE_OUTER_BOUND('',#1154,.T.);
#818=FACE_OUTER_BOUND('',#1155,.T.);
#819=FACE_OUTER_BOUND('',#1156,.T.);
#820=FACE_OUTER_BOUND('',#1157,.T.);
#821=FACE_OUTER_BOUND('',#1158,.T.);
#822=FACE_OUTER_BOUND('',#1159,.T.);
#823=FACE_OUTER_BOUND('',#1160,.T.);
#824=FACE_OUTER_BOUND('',#1162,.T.);
#825=FACE_OUTER_BOUND('',#1164,.T.);
#826=FACE_OUTER_BOUND('',#1165,.T.);
#827=FACE_OUTER_BOUND('',#1166,.T.);
#828=FACE_OUTER_BOUND('',#1167,.T.);
#829=FACE_OUTER_BOUND('',#1168,.T.);
#830=FACE_OUTER_BOUND('',#1170,.T.);
#831=FACE_OUTER_BOUND('',#1171,.T.);
#832=FACE_OUTER_BOUND('',#1172,.T.);
#833=FACE_OUTER_BOUND('',#1173,.T.);
#834=FACE_OUTER_BOUND('',#1174,.T.);
#835=FACE_OUTER_BOUND('',#1175,.T.);
#836=FACE_OUTER_BOUND('',#1176,.T.);
#837=FACE_OUTER_BOUND('',#1177,.T.);
#838=FACE_OUTER_BOUND('',#1178,.T.);
#839=FACE_OUTER_BOUND('',#1179,.T.);
#840=FACE_OUTER_BOUND('',#1180,.T.);
#841=FACE_OUTER_BOUND('',#1181,.T.);
#842=EDGE_LOOP('',(#3360,#3361,#3362,#3363));
#843=EDGE_LOOP('',(#3364,#3365,#3366,#3367));
#844=EDGE_LOOP('',(#3368,#3369,#3370,#3371));
#845=EDGE_LOOP('',(#3372,#3373,#3374,#3375));
#846=EDGE_LOOP('',(#3376,#3377,#3378,#3379));
#847=EDGE_LOOP('',(#3380,#3381,#3382,#3383));
#848=EDGE_LOOP('',(#3384,#3385,#3386,#3387));
#849=EDGE_LOOP('',(#3388,#3389,#3390,#3391));
#850=EDGE_LOOP('',(#3392,#3393,#3394,#3395));
#851=EDGE_LOOP('',(#3396,#3397,#3398,#3399));
#852=EDGE_LOOP('',(#3400,#3401,#3402,#3403));
#853=EDGE_LOOP('',(#3404,#3405,#3406,#3407));
#854=EDGE_LOOP('',(#3408,#3409,#3410,#3411));
#855=EDGE_LOOP('',(#3412,#3413,#3414,#3415));
#856=EDGE_LOOP('',(#3416,#3417,#3418,#3419));
#857=EDGE_LOOP('',(#3420,#3421,#3422,#3423));
#858=EDGE_LOOP('',(#3424,#3425,#3426,#3427));
#859=EDGE_LOOP('',(#3428,#3429,#3430,#3431));
#860=EDGE_LOOP('',(#3432,#3433,#3434,#3435));
#861=EDGE_LOOP('',(#3436));
#862=EDGE_LOOP('',(#3437));
#863=EDGE_LOOP('',(#3438));
#864=EDGE_LOOP('',(#3439));
#865=EDGE_LOOP('',(#3440));
#866=EDGE_LOOP('',(#3441));
#867=EDGE_LOOP('',(#3442));
#868=EDGE_LOOP('',(#3443));
#869=EDGE_LOOP('',(#3444));
#870=EDGE_LOOP('',(#3445));
#871=EDGE_LOOP('',(#3446));
#872=EDGE_LOOP('',(#3447));
#873=EDGE_LOOP('',(#3448));
#874=EDGE_LOOP('',(#3449));
#875=EDGE_LOOP('',(#3450,#3451,#3452,#3453));
#876=EDGE_LOOP('',(#3454));
#877=EDGE_LOOP('',(#3455));
#878=EDGE_LOOP('',(#3456));
#879=EDGE_LOOP('',(#3457));
#880=EDGE_LOOP('',(#3458));
#881=EDGE_LOOP('',(#3459));
#882=EDGE_LOOP('',(#3460));
#883=EDGE_LOOP('',(#3461));
#884=EDGE_LOOP('',(#3462));
#885=EDGE_LOOP('',(#3463));
#886=EDGE_LOOP('',(#3464));
#887=EDGE_LOOP('',(#3465));
#888=EDGE_LOOP('',(#3466));
#889=EDGE_LOOP('',(#3467));
#890=EDGE_LOOP('',(#3468,#3469,#3470,#3471));
#891=EDGE_LOOP('',(#3472,#3473,#3474,#3475));
#892=EDGE_LOOP('',(#3476,#3477,#3478,#3479));
#893=EDGE_LOOP('',(#3480,#3481,#3482,#3483));
#894=EDGE_LOOP('',(#3484,#3485,#3486,#3487));
#895=EDGE_LOOP('',(#3488,#3489,#3490,#3491));
#896=EDGE_LOOP('',(#3492,#3493,#3494,#3495));
#897=EDGE_LOOP('',(#3496,#3497,#3498,#3499));
#898=EDGE_LOOP('',(#3500,#3501,#3502,#3503));
#899=EDGE_LOOP('',(#3504,#3505,#3506,#3507));
#900=EDGE_LOOP('',(#3508,#3509,#3510,#3511));
#901=EDGE_LOOP('',(#3512,#3513,#3514,#3515));
#902=EDGE_LOOP('',(#3516,#3517,#3518,#3519));
#903=EDGE_LOOP('',(#3520,#3521,#3522,#3523));
#904=EDGE_LOOP('',(#3524,#3525,#3526,#3527));
#905=EDGE_LOOP('',(#3528,#3529,#3530,#3531));
#906=EDGE_LOOP('',(#3532,#3533,#3534,#3535));
#907=EDGE_LOOP('',(#3536,#3537,#3538,#3539));
#908=EDGE_LOOP('',(#3540,#3541,#3542,#3543));
#909=EDGE_LOOP('',(#3544,#3545,#3546,#3547));
#910=EDGE_LOOP('',(#3548,#3549,#3550,#3551));
#911=EDGE_LOOP('',(#3552,#3553,#3554,#3555));
#912=EDGE_LOOP('',(#3556,#3557,#3558,#3559));
#913=EDGE_LOOP('',(#3560,#3561,#3562,#3563));
#914=EDGE_LOOP('',(#3564,#3565,#3566,#3567));
#915=EDGE_LOOP('',(#3568,#3569,#3570,#3571));
#916=EDGE_LOOP('',(#3572,#3573,#3574,#3575));
#917=EDGE_LOOP('',(#3576,#3577,#3578,#3579));
#918=EDGE_LOOP('',(#3580,#3581,#3582,#3583));
#919=EDGE_LOOP('',(#3584,#3585,#3586,#3587));
#920=EDGE_LOOP('',(#3588,#3589,#3590,#3591));
#921=EDGE_LOOP('',(#3592,#3593,#3594,#3595));
#922=EDGE_LOOP('',(#3596,#3597,#3598,#3599));
#923=EDGE_LOOP('',(#3600,#3601,#3602,#3603));
#924=EDGE_LOOP('',(#3604,#3605,#3606,#3607));
#925=EDGE_LOOP('',(#3608,#3609,#3610,#3611));
#926=EDGE_LOOP('',(#3612,#3613,#3614,#3615));
#927=EDGE_LOOP('',(#3616,#3617,#3618,#3619));
#928=EDGE_LOOP('',(#3620,#3621,#3622,#3623));
#929=EDGE_LOOP('',(#3624,#3625,#3626,#3627));
#930=EDGE_LOOP('',(#3628,#3629,#3630,#3631));
#931=EDGE_LOOP('',(#3632,#3633,#3634,#3635));
#932=EDGE_LOOP('',(#3636,#3637,#3638,#3639));
#933=EDGE_LOOP('',(#3640,#3641,#3642,#3643));
#934=EDGE_LOOP('',(#3644,#3645,#3646,#3647));
#935=EDGE_LOOP('',(#3648,#3649,#3650,#3651,#3652,#3653,#3654,#3655,#3656,
#3657,#3658,#3659,#3660,#3661,#3662,#3663,#3664,#3665,#3666,#3667,#3668,
#3669,#3670,#3671,#3672,#3673,#3674,#3675,#3676,#3677,#3678,#3679,#3680,
#3681,#3682,#3683,#3684,#3685,#3686,#3687,#3688,#3689,#3690,#3691));
#936=EDGE_LOOP('',(#3692));
#937=EDGE_LOOP('',(#3693,#3694,#3695,#3696,#3697,#3698,#3699,#3700,#3701,
#3702,#3703,#3704,#3705,#3706,#3707,#3708,#3709,#3710,#3711,#3712,#3713,
#3714,#3715,#3716,#3717,#3718,#3719,#3720,#3721,#3722,#3723,#3724,#3725,
#3726,#3727,#3728,#3729,#3730,#3731,#3732,#3733,#3734,#3735,#3736));
#938=EDGE_LOOP('',(#3737));
#939=EDGE_LOOP('',(#3738,#3739,#3740,#3741));
#940=EDGE_LOOP('',(#3742,#3743,#3744,#3745));
#941=EDGE_LOOP('',(#3746,#3747,#3748,#3749));
#942=EDGE_LOOP('',(#3750));
#943=EDGE_LOOP('',(#3751,#3752,#3753,#3754,#3755,#3756,#3757,#3758,#3759,
#3760));
#944=EDGE_LOOP('',(#3761,#3762,#3763,#3764));
#945=EDGE_LOOP('',(#3765,#3766,#3767,#3768));
#946=EDGE_LOOP('',(#3769,#3770,#3771,#3772,#3773,#3774,#3775,#3776,#3777,
#3778));
#947=EDGE_LOOP('',(#3779,#3780,#3781,#3782));
#948=EDGE_LOOP('',(#3783,#3784,#3785,#3786,#3787,#3788));
#949=EDGE_LOOP('',(#3789,#3790,#3791,#3792,#3793,#3794,#3795,#3796));
#950=EDGE_LOOP('',(#3797,#3798,#3799,#3800,#3801));
#951=EDGE_LOOP('',(#3802,#3803,#3804,#3805));
#952=EDGE_LOOP('',(#3806,#3807,#3808,#3809,#3810,#3811));
#953=EDGE_LOOP('',(#3812,#3813,#3814,#3815));
#954=EDGE_LOOP('',(#3816,#3817,#3818,#3819));
#955=EDGE_LOOP('',(#3820,#3821,#3822,#3823));
#956=EDGE_LOOP('',(#3824,#3825,#3826,#3827));
#957=EDGE_LOOP('',(#3828,#3829,#3830,#3831));
#958=EDGE_LOOP('',(#3832,#3833,#3834,#3835));
#959=EDGE_LOOP('',(#3836,#3837,#3838,#3839));
#960=EDGE_LOOP('',(#3840,#3841,#3842,#3843,#3844,#3845));
#961=EDGE_LOOP('',(#3846,#3847,#3848,#3849,#3850,#3851));
#962=EDGE_LOOP('',(#3852));
#963=EDGE_LOOP('',(#3853));
#964=EDGE_LOOP('',(#3854,#3855,#3856,#3857));
#965=EDGE_LOOP('',(#3858,#3859,#3860,#3861));
#966=EDGE_LOOP('',(#3862,#3863,#3864,#3865));
#967=EDGE_LOOP('',(#3866));
#968=EDGE_LOOP('',(#3867));
#969=EDGE_LOOP('',(#3868,#3869,#3870,#3871));
#970=EDGE_LOOP('',(#3872,#3873,#3874,#3875));
#971=EDGE_LOOP('',(#3876,#3877,#3878,#3879));
#972=EDGE_LOOP('',(#3880));
#973=EDGE_LOOP('',(#3881));
#974=EDGE_LOOP('',(#3882,#3883,#3884,#3885));
#975=EDGE_LOOP('',(#3886));
#976=EDGE_LOOP('',(#3887));
#977=EDGE_LOOP('',(#3888,#3889,#3890,#3891));
#978=EDGE_LOOP('',(#3892));
#979=EDGE_LOOP('',(#3893));
#980=EDGE_LOOP('',(#3894,#3895,#3896,#3897));
#981=EDGE_LOOP('',(#3898));
#982=EDGE_LOOP('',(#3899));
#983=EDGE_LOOP('',(#3900,#3901,#3902,#3903));
#984=EDGE_LOOP('',(#3904,#3905,#3906,#3907));
#985=EDGE_LOOP('',(#3908,#3909,#3910,#3911));
#986=EDGE_LOOP('',(#3912,#3913,#3914,#3915));
#987=EDGE_LOOP('',(#3916,#3917,#3918,#3919));
#988=EDGE_LOOP('',(#3920,#3921,#3922,#3923));
#989=EDGE_LOOP('',(#3924,#3925,#3926,#3927));
#990=EDGE_LOOP('',(#3928,#3929,#3930,#3931));
#991=EDGE_LOOP('',(#3932,#3933,#3934,#3935));
#992=EDGE_LOOP('',(#3936));
#993=EDGE_LOOP('',(#3937));
#994=EDGE_LOOP('',(#3938));
#995=EDGE_LOOP('',(#3939));
#996=EDGE_LOOP('',(#3940,#3941,#3942,#3943));
#997=EDGE_LOOP('',(#3944,#3945,#3946,#3947));
#998=EDGE_LOOP('',(#3948,#3949,#3950,#3951));
#999=EDGE_LOOP('',(#3952,#3953,#3954,#3955));
#1000=EDGE_LOOP('',(#3956,#3957,#3958,#3959));
#1001=EDGE_LOOP('',(#3960,#3961,#3962,#3963));
#1002=EDGE_LOOP('',(#3964));
#1003=EDGE_LOOP('',(#3965));
#1004=EDGE_LOOP('',(#3966));
#1005=EDGE_LOOP('',(#3967));
#1006=EDGE_LOOP('',(#3968,#3969,#3970,#3971));
#1007=EDGE_LOOP('',(#3972,#3973,#3974,#3975,#3976,#3977,#3978,#3979,#3980,
#3981,#3982,#3983));
#1008=EDGE_LOOP('',(#3984,#3985,#3986,#3987,#3988,#3989,#3990,#3991,#3992,
#3993,#3994,#3995));
#1009=EDGE_LOOP('',(#3996));
#1010=EDGE_LOOP('',(#3997,#3998,#3999,#4000));
#1011=EDGE_LOOP('',(#4001,#4002,#4003,#4004));
#1012=EDGE_LOOP('',(#4005,#4006,#4007,#4008));
#1013=EDGE_LOOP('',(#4009));
#1014=EDGE_LOOP('',(#4010));
#1015=EDGE_LOOP('',(#4011,#4012,#4013,#4014));
#1016=EDGE_LOOP('',(#4015,#4016,#4017,#4018));
#1017=EDGE_LOOP('',(#4019,#4020,#4021,#4022));
#1018=EDGE_LOOP('',(#4023));
#1019=EDGE_LOOP('',(#4024,#4025,#4026,#4027));
#1020=EDGE_LOOP('',(#4028,#4029,#4030,#4031));
#1021=EDGE_LOOP('',(#4032,#4033,#4034,#4035));
#1022=EDGE_LOOP('',(#4036,#4037,#4038,#4039));
#1023=EDGE_LOOP('',(#4040,#4041,#4042,#4043));
#1024=EDGE_LOOP('',(#4044,#4045,#4046,#4047));
#1025=EDGE_LOOP('',(#4048,#4049,#4050,#4051,#4052,#4053));
#1026=EDGE_LOOP('',(#4054,#4055,#4056,#4057,#4058,#4059));
#1027=EDGE_LOOP('',(#4060,#4061,#4062,#4063));
#1028=EDGE_LOOP('',(#4064));
#1029=EDGE_LOOP('',(#4065));
#1030=EDGE_LOOP('',(#4066,#4067,#4068,#4069));
#1031=EDGE_LOOP('',(#4070));
#1032=EDGE_LOOP('',(#4071));
#1033=EDGE_LOOP('',(#4072,#4073,#4074,#4075));
#1034=EDGE_LOOP('',(#4076,#4077,#4078,#4079));
#1035=EDGE_LOOP('',(#4080,#4081,#4082,#4083));
#1036=EDGE_LOOP('',(#4084,#4085,#4086,#4087));
#1037=EDGE_LOOP('',(#4088,#4089,#4090,#4091));
#1038=EDGE_LOOP('',(#4092,#4093,#4094,#4095));
#1039=EDGE_LOOP('',(#4096,#4097,#4098,#4099));
#1040=EDGE_LOOP('',(#4100));
#1041=EDGE_LOOP('',(#4101));
#1042=EDGE_LOOP('',(#4102,#4103,#4104,#4105));
#1043=EDGE_LOOP('',(#4106));
#1044=EDGE_LOOP('',(#4107));
#1045=EDGE_LOOP('',(#4108,#4109,#4110,#4111));
#1046=EDGE_LOOP('',(#4112,#4113,#4114,#4115));
#1047=EDGE_LOOP('',(#4116,#4117,#4118,#4119));
#1048=EDGE_LOOP('',(#4120,#4121,#4122,#4123));
#1049=EDGE_LOOP('',(#4124,#4125,#4126,#4127));
#1050=EDGE_LOOP('',(#4128,#4129,#4130,#4131));
#1051=EDGE_LOOP('',(#4132,#4133,#4134,#4135));
#1052=EDGE_LOOP('',(#4136,#4137,#4138,#4139));
#1053=EDGE_LOOP('',(#4140,#4141,#4142,#4143));
#1054=EDGE_LOOP('',(#4144,#4145,#4146,#4147));
#1055=EDGE_LOOP('',(#4148,#4149,#4150,#4151));
#1056=EDGE_LOOP('',(#4152,#4153,#4154,#4155));
#1057=EDGE_LOOP('',(#4156,#4157));
#1058=EDGE_LOOP('',(#4158,#4159,#4160,#4161,#4162,#4163,#4164,#4165));
#1059=EDGE_LOOP('',(#4166,#4167));
#1060=EDGE_LOOP('',(#4168,#4169,#4170,#4171,#4172,#4173,#4174,#4175));
#1061=EDGE_LOOP('',(#4176,#4177));
#1062=EDGE_LOOP('',(#4178,#4179,#4180,#4181,#4182,#4183,#4184,#4185));
#1063=EDGE_LOOP('',(#4186,#4187));
#1064=EDGE_LOOP('',(#4188,#4189,#4190,#4191,#4192,#4193,#4194,#4195));
#1065=EDGE_LOOP('',(#4196,#4197,#4198,#4199,#4200,#4201,#4202,#4203,#4204,
#4205,#4206,#4207));
#1066=EDGE_LOOP('',(#4208,#4209,#4210,#4211,#4212,#4213,#4214,#4215,#4216,
#4217,#4218,#4219));
#1067=EDGE_LOOP('',(#4220,#4221,#4222,#4223,#4224,#4225,#4226,#4227,#4228,
#4229,#4230,#4231));
#1068=EDGE_LOOP('',(#4232,#4233,#4234,#4235,#4236,#4237,#4238,#4239,#4240,
#4241));
#1069=EDGE_LOOP('',(#4242,#4243,#4244,#4245));
#1070=EDGE_LOOP('',(#4246,#4247,#4248,#4249));
#1071=EDGE_LOOP('',(#4250));
#1072=EDGE_LOOP('',(#4251));
#1073=EDGE_LOOP('',(#4252));
#1074=EDGE_LOOP('',(#4253));
#1075=EDGE_LOOP('',(#4254,#4255,#4256,#4257));
#1076=EDGE_LOOP('',(#4258,#4259,#4260,#4261,#4262,#4263,#4264,#4265,#4266,
#4267));
#1077=EDGE_LOOP('',(#4268,#4269,#4270,#4271));
#1078=EDGE_LOOP('',(#4272,#4273,#4274,#4275));
#1079=EDGE_LOOP('',(#4276,#4277,#4278,#4279));
#1080=EDGE_LOOP('',(#4280,#4281,#4282,#4283));
#1081=EDGE_LOOP('',(#4284,#4285,#4286,#4287));
#1082=EDGE_LOOP('',(#4288,#4289,#4290,#4291,#4292,#4293,#4294,#4295,#4296,
#4297,#4298,#4299));
#1083=EDGE_LOOP('',(#4300,#4301,#4302,#4303));
#1084=EDGE_LOOP('',(#4304,#4305,#4306,#4307));
#1085=EDGE_LOOP('',(#4308,#4309,#4310,#4311));
#1086=EDGE_LOOP('',(#4312,#4313,#4314,#4315));
#1087=EDGE_LOOP('',(#4316,#4317,#4318,#4319));
#1088=EDGE_LOOP('',(#4320,#4321,#4322,#4323));
#1089=EDGE_LOOP('',(#4324,#4325,#4326,#4327));
#1090=EDGE_LOOP('',(#4328,#4329,#4330,#4331));
#1091=EDGE_LOOP('',(#4332,#4333,#4334,#4335,#4336,#4337,#4338,#4339));
#1092=EDGE_LOOP('',(#4340,#4341,#4342,#4343,#4344,#4345,#4346,#4347));
#1093=EDGE_LOOP('',(#4348,#4349,#4350,#4351));
#1094=EDGE_LOOP('',(#4352,#4353,#4354,#4355));
#1095=EDGE_LOOP('',(#4356,#4357,#4358,#4359));
#1096=EDGE_LOOP('',(#4360,#4361,#4362,#4363));
#1097=EDGE_LOOP('',(#4364,#4365,#4366,#4367));
#1098=EDGE_LOOP('',(#4368,#4369,#4370,#4371));
#1099=EDGE_LOOP('',(#4372,#4373,#4374,#4375));
#1100=EDGE_LOOP('',(#4376,#4377,#4378,#4379));
#1101=EDGE_LOOP('',(#4380,#4381,#4382,#4383,#4384,#4385,#4386,#4387));
#1102=EDGE_LOOP('',(#4388,#4389,#4390,#4391,#4392,#4393,#4394,#4395));
#1103=EDGE_LOOP('',(#4396,#4397,#4398,#4399));
#1104=EDGE_LOOP('',(#4400,#4401,#4402,#4403));
#1105=EDGE_LOOP('',(#4404,#4405,#4406,#4407));
#1106=EDGE_LOOP('',(#4408,#4409,#4410,#4411));
#1107=EDGE_LOOP('',(#4412,#4413,#4414,#4415));
#1108=EDGE_LOOP('',(#4416,#4417,#4418,#4419));
#1109=EDGE_LOOP('',(#4420,#4421,#4422,#4423));
#1110=EDGE_LOOP('',(#4424,#4425,#4426,#4427));
#1111=EDGE_LOOP('',(#4428,#4429,#4430,#4431));
#1112=EDGE_LOOP('',(#4432,#4433,#4434,#4435));
#1113=EDGE_LOOP('',(#4436,#4437,#4438,#4439));
#1114=EDGE_LOOP('',(#4440));
#1115=EDGE_LOOP('',(#4441));
#1116=EDGE_LOOP('',(#4442));
#1117=EDGE_LOOP('',(#4443));
#1118=EDGE_LOOP('',(#4444));
#1119=EDGE_LOOP('',(#4445));
#1120=EDGE_LOOP('',(#4446,#4447,#4448,#4449));
#1121=EDGE_LOOP('',(#4450));
#1122=EDGE_LOOP('',(#4451));
#1123=EDGE_LOOP('',(#4452));
#1124=EDGE_LOOP('',(#4453));
#1125=EDGE_LOOP('',(#4454));
#1126=EDGE_LOOP('',(#4455));
#1127=EDGE_LOOP('',(#4456,#4457,#4458,#4459));
#1128=EDGE_LOOP('',(#4460,#4461,#4462,#4463));
#1129=EDGE_LOOP('',(#4464));
#1130=EDGE_LOOP('',(#4465));
#1131=EDGE_LOOP('',(#4466));
#1132=EDGE_LOOP('',(#4467));
#1133=EDGE_LOOP('',(#4468,#4469,#4470,#4471));
#1134=EDGE_LOOP('',(#4472,#4473,#4474,#4475));
#1135=EDGE_LOOP('',(#4476));
#1136=EDGE_LOOP('',(#4477));
#1137=EDGE_LOOP('',(#4478,#4479,#4480,#4481));
#1138=EDGE_LOOP('',(#4482));
#1139=EDGE_LOOP('',(#4483));
#1140=EDGE_LOOP('',(#4484));
#1141=EDGE_LOOP('',(#4485,#4486,#4487,#4488));
#1142=EDGE_LOOP('',(#4489,#4490,#4491,#4492));
#1143=EDGE_LOOP('',(#4493,#4494,#4495,#4496));
#1144=EDGE_LOOP('',(#4497));
#1145=EDGE_LOOP('',(#4498));
#1146=EDGE_LOOP('',(#4499,#4500,#4501,#4502));
#1147=EDGE_LOOP('',(#4503,#4504,#4505,#4506));
#1148=EDGE_LOOP('',(#4507,#4508,#4509,#4510));
#1149=EDGE_LOOP('',(#4511));
#1150=EDGE_LOOP('',(#4512,#4513,#4514,#4515));
#1151=EDGE_LOOP('',(#4516,#4517,#4518,#4519));
#1152=EDGE_LOOP('',(#4520,#4521,#4522,#4523));
#1153=EDGE_LOOP('',(#4524,#4525,#4526,#4527));
#1154=EDGE_LOOP('',(#4528,#4529,#4530,#4531));
#1155=EDGE_LOOP('',(#4532,#4533,#4534,#4535));
#1156=EDGE_LOOP('',(#4536,#4537,#4538,#4539,#4540,#4541));
#1157=EDGE_LOOP('',(#4542,#4543,#4544,#4545,#4546,#4547));
#1158=EDGE_LOOP('',(#4548,#4549,#4550,#4551));
#1159=EDGE_LOOP('',(#4552,#4553,#4554,#4555));
#1160=EDGE_LOOP('',(#4556));
#1161=EDGE_LOOP('',(#4557));
#1162=EDGE_LOOP('',(#4558));
#1163=EDGE_LOOP('',(#4559));
#1164=EDGE_LOOP('',(#4560));
#1165=EDGE_LOOP('',(#4561,#4562,#4563,#4564));
#1166=EDGE_LOOP('',(#4565,#4566,#4567,#4568));
#1167=EDGE_LOOP('',(#4569,#4570,#4571,#4572));
#1168=EDGE_LOOP('',(#4573));
#1169=EDGE_LOOP('',(#4574));
#1170=EDGE_LOOP('',(#4575,#4576,#4577,#4578));
#1171=EDGE_LOOP('',(#4579,#4580,#4581,#4582));
#1172=EDGE_LOOP('',(#4583,#4584,#4585,#4586));
#1173=EDGE_LOOP('',(#4587));
#1174=EDGE_LOOP('',(#4588,#4589,#4590,#4591));
#1175=EDGE_LOOP('',(#4592,#4593,#4594,#4595));
#1176=EDGE_LOOP('',(#4596,#4597,#4598,#4599));
#1177=EDGE_LOOP('',(#4600,#4601,#4602,#4603));
#1178=EDGE_LOOP('',(#4604,#4605,#4606,#4607));
#1179=EDGE_LOOP('',(#4608,#4609,#4610,#4611));
#1180=EDGE_LOOP('',(#4612,#4613,#4614,#4615,#4616,#4617));
#1181=EDGE_LOOP('',(#4618,#4619,#4620,#4621,#4622,#4623));
#1182=LINE('',#7076,#1682);
#1183=LINE('',#7082,#1683);
#1184=LINE('',#7088,#1684);
#1185=LINE('',#7094,#1685);
#1186=LINE('',#7100,#1686);
#1187=LINE('',#7106,#1687);
#1188=LINE('',#7112,#1688);
#1189=LINE('',#7118,#1689);
#1190=LINE('',#7124,#1690);
#1191=LINE('',#7130,#1691);
#1192=LINE('',#7136,#1692);
#1193=LINE('',#7142,#1693);
#1194=LINE('',#7148,#1694);
#1195=LINE('',#7154,#1695);
#1196=LINE('',#7159,#1696);
#1197=LINE('',#7161,#1697);
#1198=LINE('',#7163,#1698);
#1199=LINE('',#7164,#1699);
#1200=LINE('',#7167,#1700);
#1201=LINE('',#7169,#1701);
#1202=LINE('',#7170,#1702);
#1203=LINE('',#7173,#1703);
#1204=LINE('',#7175,#1704);
#1205=LINE('',#7176,#1705);
#1206=LINE('',#7178,#1706);
#1207=LINE('',#7179,#1707);
#1208=LINE('',#7186,#1708);
#1209=LINE('',#7188,#1709);
#1210=LINE('',#7190,#1710);
#1211=LINE('',#7191,#1711);
#1212=LINE('',#7194,#1712);
#1213=LINE('',#7196,#1713);
#1214=LINE('',#7197,#1714);
#1215=LINE('',#7200,#1715);
#1216=LINE('',#7202,#1716);
#1217=LINE('',#7203,#1717);
#1218=LINE('',#7206,#1718);
#1219=LINE('',#7208,#1719);
#1220=LINE('',#7209,#1720);
#1221=LINE('',#7212,#1721);
#1222=LINE('',#7214,#1722);
#1223=LINE('',#7215,#1723);
#1224=LINE('',#7218,#1724);
#1225=LINE('',#7220,#1725);
#1226=LINE('',#7221,#1726);
#1227=LINE('',#7224,#1727);
#1228=LINE('',#7226,#1728);
#1229=LINE('',#7227,#1729);
#1230=LINE('',#7230,#1730);
#1231=LINE('',#7232,#1731);
#1232=LINE('',#7233,#1732);
#1233=LINE('',#7236,#1733);
#1234=LINE('',#7238,#1734);
#1235=LINE('',#7239,#1735);
#1236=LINE('',#7243,#1736);
#1237=LINE('',#7245,#1737);
#1238=LINE('',#7247,#1738);
#1239=LINE('',#7248,#1739);
#1240=LINE('',#7251,#1740);
#1241=LINE('',#7253,#1741);
#1242=LINE('',#7254,#1742);
#1243=LINE('',#7257,#1743);
#1244=LINE('',#7259,#1744);
#1245=LINE('',#7260,#1745);
#1246=LINE('',#7263,#1746);
#1247=LINE('',#7265,#1747);
#1248=LINE('',#7266,#1748);
#1249=LINE('',#7269,#1749);
#1250=LINE('',#7271,#1750);
#1251=LINE('',#7272,#1751);
#1252=LINE('',#7275,#1752);
#1253=LINE('',#7277,#1753);
#1254=LINE('',#7278,#1754);
#1255=LINE('',#7281,#1755);
#1256=LINE('',#7283,#1756);
#1257=LINE('',#7284,#1757);
#1258=LINE('',#7287,#1758);
#1259=LINE('',#7289,#1759);
#1260=LINE('',#7290,#1760);
#1261=LINE('',#7293,#1761);
#1262=LINE('',#7295,#1762);
#1263=LINE('',#7296,#1763);
#1264=LINE('',#7300,#1764);
#1265=LINE('',#7302,#1765);
#1266=LINE('',#7304,#1766);
#1267=LINE('',#7305,#1767);
#1268=LINE('',#7308,#1768);
#1269=LINE('',#7310,#1769);
#1270=LINE('',#7311,#1770);
#1271=LINE('',#7314,#1771);
#1272=LINE('',#7316,#1772);
#1273=LINE('',#7317,#1773);
#1274=LINE('',#7320,#1774);
#1275=LINE('',#7322,#1775);
#1276=LINE('',#7323,#1776);
#1277=LINE('',#7326,#1777);
#1278=LINE('',#7328,#1778);
#1279=LINE('',#7329,#1779);
#1280=LINE('',#7332,#1780);
#1281=LINE('',#7334,#1781);
#1282=LINE('',#7335,#1782);
#1283=LINE('',#7338,#1783);
#1284=LINE('',#7340,#1784);
#1285=LINE('',#7341,#1785);
#1286=LINE('',#7344,#1786);
#1287=LINE('',#7346,#1787);
#1288=LINE('',#7347,#1788);
#1289=LINE('',#7350,#1789);
#1290=LINE('',#7352,#1790);
#1291=LINE('',#7353,#1791);
#1292=LINE('',#7357,#1792);
#1293=LINE('',#7359,#1793);
#1294=LINE('',#7361,#1794);
#1295=LINE('',#7362,#1795);
#1296=LINE('',#7365,#1796);
#1297=LINE('',#7367,#1797);
#1298=LINE('',#7368,#1798);
#1299=LINE('',#7371,#1799);
#1300=LINE('',#7373,#1800);
#1301=LINE('',#7374,#1801);
#1302=LINE('',#7377,#1802);
#1303=LINE('',#7379,#1803);
#1304=LINE('',#7380,#1804);
#1305=LINE('',#7383,#1805);
#1306=LINE('',#7385,#1806);
#1307=LINE('',#7386,#1807);
#1308=LINE('',#7389,#1808);
#1309=LINE('',#7391,#1809);
#1310=LINE('',#7392,#1810);
#1311=LINE('',#7395,#1811);
#1312=LINE('',#7397,#1812);
#1313=LINE('',#7398,#1813);
#1314=LINE('',#7401,#1814);
#1315=LINE('',#7403,#1815);
#1316=LINE('',#7404,#1816);
#1317=LINE('',#7407,#1817);
#1318=LINE('',#7409,#1818);
#1319=LINE('',#7410,#1819);
#1320=LINE('',#7415,#1820);
#1321=LINE('',#7419,#1821);
#1322=LINE('',#7421,#1822);
#1323=LINE('',#7422,#1823);
#1324=LINE('',#7425,#1824);
#1325=LINE('',#7427,#1825);
#1326=LINE('',#7428,#1826);
#1327=LINE('',#7430,#1827);
#1328=LINE('',#7431,#1828);
#1329=LINE('',#7434,#1829);
#1330=LINE('',#7436,#1830);
#1331=LINE('',#7437,#1831);
#1332=LINE('',#7439,#1832);
#1333=LINE('',#7440,#1833);
#1334=LINE('',#7443,#1834);
#1335=LINE('',#7445,#1835);
#1336=LINE('',#7446,#1836);
#1337=LINE('',#7448,#1837);
#1338=LINE('',#7449,#1838);
#1339=LINE('',#7451,#1839);
#1340=LINE('',#7452,#1840);
#1341=LINE('',#7459,#1841);
#1342=LINE('',#7461,#1842);
#1343=LINE('',#7463,#1843);
#1344=LINE('',#7464,#1844);
#1345=LINE('',#7467,#1845);
#1346=LINE('',#7469,#1846);
#1347=LINE('',#7470,#1847);
#1348=LINE('',#7473,#1848);
#1349=LINE('',#7475,#1849);
#1350=LINE('',#7476,#1850);
#1351=LINE('',#7481,#1851);
#1352=LINE('',#7483,#1852);
#1353=LINE('',#7485,#1853);
#1354=LINE('',#7487,#1854);
#1355=LINE('',#7489,#1855);
#1356=LINE('',#7491,#1856);
#1357=LINE('',#7492,#1857);
#1358=LINE('',#7495,#1858);
#1359=LINE('',#7496,#1859);
#1360=LINE('',#7499,#1860);
#1361=LINE('',#7500,#1861);
#1362=LINE('',#7503,#1862);
#1363=LINE('',#7505,#1863);
#1364=LINE('',#7507,#1864);
#1365=LINE('',#7509,#1865);
#1366=LINE('',#7510,#1866);
#1367=LINE('',#7512,#1867);
#1368=LINE('',#7515,#1868);
#1369=LINE('',#7518,#1869);
#1370=LINE('',#7522,#1870);
#1371=LINE('',#7529,#1871);
#1372=LINE('',#7531,#1872);
#1373=LINE('',#7533,#1873);
#1374=LINE('',#7539,#1874);
#1375=LINE('',#7541,#1875);
#1376=LINE('',#7543,#1876);
#1377=LINE('',#7544,#1877);
#1378=LINE('',#7547,#1878);
#1379=LINE('',#7549,#1879);
#1380=LINE('',#7550,#1880);
#1381=LINE('',#7553,#1881);
#1382=LINE('',#7555,#1882);
#1383=LINE('',#7556,#1883);
#1384=LINE('',#7559,#1884);
#1385=LINE('',#7561,#1885);
#1386=LINE('',#7562,#1886);
#1387=LINE('',#7565,#1887);
#1388=LINE('',#7567,#1888);
#1389=LINE('',#7568,#1889);
#1390=LINE('',#7570,#1890);
#1391=LINE('',#7571,#1891);
#1392=LINE('',#7583,#1892);
#1393=LINE('',#7587,#1893);
#1394=LINE('',#7591,#1894);
#1395=LINE('',#7598,#1895);
#1396=LINE('',#7600,#1896);
#1397=LINE('',#7606,#1897);
#1398=LINE('',#7615,#1898);
#1399=LINE('',#7624,#1899);
#1400=LINE('',#7633,#1900);
#1401=LINE('',#7641,#1901);
#1402=LINE('',#7645,#1902);
#1403=LINE('',#7649,#1903);
#1404=LINE('',#7653,#1904);
#1405=LINE('',#7657,#1905);
#1406=LINE('',#7659,#1906);
#1407=LINE('',#7661,#1907);
#1408=LINE('',#7662,#1908);
#1409=LINE('',#7665,#1909);
#1410=LINE('',#7667,#1910);
#1411=LINE('',#7668,#1911);
#1412=LINE('',#7671,#1912);
#1413=LINE('',#7673,#1913);
#1414=LINE('',#7674,#1914);
#1415=LINE('',#7677,#1915);
#1416=LINE('',#7679,#1916);
#1417=LINE('',#7680,#1917);
#1418=LINE('',#7683,#1918);
#1419=LINE('',#7685,#1919);
#1420=LINE('',#7686,#1920);
#1421=LINE('',#7689,#1921);
#1422=LINE('',#7691,#1922);
#1423=LINE('',#7692,#1923);
#1424=LINE('',#7695,#1924);
#1425=LINE('',#7697,#1925);
#1426=LINE('',#7698,#1926);
#1427=LINE('',#7701,#1927);
#1428=LINE('',#7703,#1928);
#1429=LINE('',#7704,#1929);
#1430=LINE('',#7707,#1930);
#1431=LINE('',#7709,#1931);
#1432=LINE('',#7710,#1932);
#1433=LINE('',#7713,#1933);
#1434=LINE('',#7715,#1934);
#1435=LINE('',#7716,#1935);
#1436=LINE('',#7719,#1936);
#1437=LINE('',#7721,#1937);
#1438=LINE('',#7722,#1938);
#1439=LINE('',#7724,#1939);
#1440=LINE('',#7725,#1940);
#1441=LINE('',#7735,#1941);
#1442=LINE('',#7739,#1942);
#1443=LINE('',#7743,#1943);
#1444=LINE('',#7750,#1944);
#1445=LINE('',#7754,#1945);
#1446=LINE('',#7758,#1946);
#1447=LINE('',#7763,#1947);
#1448=LINE('',#7765,#1948);
#1449=LINE('',#7767,#1949);
#1450=LINE('',#7768,#1950);
#1451=LINE('',#7771,#1951);
#1452=LINE('',#7773,#1952);
#1453=LINE('',#7774,#1953);
#1454=LINE('',#7777,#1954);
#1455=LINE('',#7779,#1955);
#1456=LINE('',#7780,#1956);
#1457=LINE('',#7783,#1957);
#1458=LINE('',#7785,#1958);
#1459=LINE('',#7786,#1959);
#1460=LINE('',#7789,#1960);
#1461=LINE('',#7791,#1961);
#1462=LINE('',#7792,#1962);
#1463=LINE('',#7794,#1963);
#1464=LINE('',#7795,#1964);
#1465=LINE('',#7803,#1965);
#1466=LINE('',#7812,#1966);
#1467=LINE('',#7820,#1967);
#1468=LINE('',#7824,#1968);
#1469=LINE('',#7828,#1969);
#1470=LINE('',#7830,#1970);
#1471=LINE('',#7832,#1971);
#1472=LINE('',#7833,#1972);
#1473=LINE('',#7836,#1973);
#1474=LINE('',#7838,#1974);
#1475=LINE('',#7839,#1975);
#1476=LINE('',#7842,#1976);
#1477=LINE('',#7844,#1977);
#1478=LINE('',#7845,#1978);
#1479=LINE('',#7847,#1979);
#1480=LINE('',#7848,#1980);
#1481=LINE('',#7855,#1981);
#1482=LINE('',#7857,#1982);
#1483=LINE('',#7859,#1983);
#1484=LINE('',#7860,#1984);
#1485=LINE('',#7863,#1985);
#1486=LINE('',#7865,#1986);
#1487=LINE('',#7866,#1987);
#1488=LINE('',#7869,#1988);
#1489=LINE('',#7871,#1989);
#1490=LINE('',#7872,#1990);
#1491=LINE('',#7874,#1991);
#1492=LINE('',#7875,#1992);
#1493=LINE('',#7882,#1993);
#1494=LINE('',#7884,#1994);
#1495=LINE('',#7886,#1995);
#1496=LINE('',#7887,#1996);
#1497=LINE('',#7890,#1997);
#1498=LINE('',#7892,#1998);
#1499=LINE('',#7893,#1999);
#1500=LINE('',#7896,#2000);
#1501=LINE('',#7898,#2001);
#1502=LINE('',#7899,#2002);
#1503=LINE('',#7901,#2003);
#1504=LINE('',#7902,#2004);
#1505=LINE('',#7911,#2005);
#1506=LINE('',#7915,#2006);
#1507=LINE('',#7919,#2007);
#1508=LINE('',#7923,#2008);
#1509=LINE('',#7927,#2009);
#1510=LINE('',#7931,#2010);
#1511=LINE('',#7935,#2011);
#1512=LINE('',#7939,#2012);
#1513=LINE('',#7943,#2013);
#1514=LINE('',#7947,#2014);
#1515=LINE('',#7951,#2015);
#1516=LINE('',#7955,#2016);
#1517=LINE('',#7959,#2017);
#1518=LINE('',#7963,#2018);
#1519=LINE('',#7967,#2019);
#1520=LINE('',#7971,#2020);
#1521=LINE('',#7973,#2021);
#1522=LINE('',#7975,#2022);
#1523=LINE('',#7977,#2023);
#1524=LINE('',#7979,#2024);
#1525=LINE('',#7981,#2025);
#1526=LINE('',#7982,#2026);
#1527=LINE('',#7984,#2027);
#1528=LINE('',#7986,#2028);
#1529=LINE('',#7988,#2029);
#1530=LINE('',#7990,#2030);
#1531=LINE('',#7992,#2031);
#1532=LINE('',#7993,#2032);
#1533=LINE('',#7996,#2033);
#1534=LINE('',#7998,#2034);
#1535=LINE('',#8000,#2035);
#1536=LINE('',#8002,#2036);
#1537=LINE('',#8003,#2037);
#1538=LINE('',#8005,#2038);
#1539=LINE('',#8007,#2039);
#1540=LINE('',#8009,#2040);
#1541=LINE('',#8011,#2041);
#1542=LINE('',#8012,#2042);
#1543=LINE('',#8015,#2043);
#1544=LINE('',#8016,#2044);
#1545=LINE('',#8019,#2045);
#1546=LINE('',#8020,#2046);
#1547=LINE('',#8023,#2047);
#1548=LINE('',#8024,#2048);
#1549=LINE('',#8027,#2049);
#1550=LINE('',#8028,#2050);
#1551=LINE('',#8030,#2051);
#1552=LINE('',#8033,#2052);
#1553=LINE('',#8034,#2053);
#1554=LINE('',#8037,#2054);
#1555=LINE('',#8038,#2055);
#1556=LINE('',#8041,#2056);
#1557=LINE('',#8042,#2057);
#1558=LINE('',#8045,#2058);
#1559=LINE('',#8046,#2059);
#1560=LINE('',#8048,#2060);
#1561=LINE('',#8054,#2061);
#1562=LINE('',#8056,#2062);
#1563=LINE('',#8058,#2063);
#1564=LINE('',#8059,#2064);
#1565=LINE('',#8062,#2065);
#1566=LINE('',#8064,#2066);
#1567=LINE('',#8065,#2067);
#1568=LINE('',#8068,#2068);
#1569=LINE('',#8070,#2069);
#1570=LINE('',#8071,#2070);
#1571=LINE('',#8074,#2071);
#1572=LINE('',#8076,#2072);
#1573=LINE('',#8077,#2073);
#1574=LINE('',#8080,#2074);
#1575=LINE('',#8082,#2075);
#1576=LINE('',#8083,#2076);
#1577=LINE('',#8086,#2077);
#1578=LINE('',#8088,#2078);
#1579=LINE('',#8089,#2079);
#1580=LINE('',#8092,#2080);
#1581=LINE('',#8094,#2081);
#1582=LINE('',#8095,#2082);
#1583=LINE('',#8097,#2083);
#1584=LINE('',#8098,#2084);
#1585=LINE('',#8105,#2085);
#1586=LINE('',#8107,#2086);
#1587=LINE('',#8109,#2087);
#1588=LINE('',#8110,#2088);
#1589=LINE('',#8113,#2089);
#1590=LINE('',#8115,#2090);
#1591=LINE('',#8116,#2091);
#1592=LINE('',#8119,#2092);
#1593=LINE('',#8121,#2093);
#1594=LINE('',#8122,#2094);
#1595=LINE('',#8125,#2095);
#1596=LINE('',#8127,#2096);
#1597=LINE('',#8128,#2097);
#1598=LINE('',#8131,#2098);
#1599=LINE('',#8133,#2099);
#1600=LINE('',#8134,#2100);
#1601=LINE('',#8137,#2101);
#1602=LINE('',#8139,#2102);
#1603=LINE('',#8140,#2103);
#1604=LINE('',#8143,#2104);
#1605=LINE('',#8145,#2105);
#1606=LINE('',#8146,#2106);
#1607=LINE('',#8148,#2107);
#1608=LINE('',#8149,#2108);
#1609=LINE('',#8160,#2109);
#1610=LINE('',#8166,#2110);
#1611=LINE('',#8172,#2111);
#1612=LINE('',#8178,#2112);
#1613=LINE('',#8184,#2113);
#1614=LINE('',#8190,#2114);
#1615=LINE('',#8195,#2115);
#1616=LINE('',#8197,#2116);
#1617=LINE('',#8199,#2117);
#1618=LINE('',#8200,#2118);
#1619=LINE('',#8203,#2119);
#1620=LINE('',#8205,#2120);
#1621=LINE('',#8206,#2121);
#1622=LINE('',#8209,#2122);
#1623=LINE('',#8211,#2123);
#1624=LINE('',#8212,#2124);
#1625=LINE('',#8214,#2125);
#1626=LINE('',#8215,#2126);
#1627=LINE('',#8223,#2127);
#1628=LINE('',#8229,#2128);
#1629=LINE('',#8238,#2129);
#1630=LINE('',#8242,#2130);
#1631=LINE('',#8249,#2131);
#1632=LINE('',#8259,#2132);
#1633=LINE('',#8263,#2133);
#1634=LINE('',#8267,#2134);
#1635=LINE('',#8274,#2135);
#1636=LINE('',#8278,#2136);
#1637=LINE('',#8282,#2137);
#1638=LINE('',#8287,#2138);
#1639=LINE('',#8289,#2139);
#1640=LINE('',#8291,#2140);
#1641=LINE('',#8292,#2141);
#1642=LINE('',#8295,#2142);
#1643=LINE('',#8297,#2143);
#1644=LINE('',#8298,#2144);
#1645=LINE('',#8301,#2145);
#1646=LINE('',#8303,#2146);
#1647=LINE('',#8304,#2147);
#1648=LINE('',#8307,#2148);
#1649=LINE('',#8309,#2149);
#1650=LINE('',#8310,#2150);
#1651=LINE('',#8313,#2151);
#1652=LINE('',#8315,#2152);
#1653=LINE('',#8316,#2153);
#1654=LINE('',#8318,#2154);
#1655=LINE('',#8319,#2155);
#1656=LINE('',#8359,#2156);
#1657=LINE('',#8365,#2157);
#1658=LINE('',#8376,#2158);
#1659=LINE('',#8380,#2159);
#1660=LINE('',#8384,#2160);
#1661=LINE('',#8391,#2161);
#1662=LINE('',#8395,#2162);
#1663=LINE('',#8399,#2163);
#1664=LINE('',#8404,#2164);
#1665=LINE('',#8406,#2165);
#1666=LINE('',#8408,#2166);
#1667=LINE('',#8409,#2167);
#1668=LINE('',#8412,#2168);
#1669=LINE('',#8414,#2169);
#1670=LINE('',#8415,#2170);
#1671=LINE('',#8418,#2171);
#1672=LINE('',#8420,#2172);
#1673=LINE('',#8421,#2173);
#1674=LINE('',#8424,#2174);
#1675=LINE('',#8426,#2175);
#1676=LINE('',#8427,#2176);
#1677=LINE('',#8430,#2177);
#1678=LINE('',#8432,#2178);
#1679=LINE('',#8433,#2179);
#1680=LINE('',#8435,#2180);
#1681=LINE('',#8436,#2181);
#1682=VECTOR('',#5641,0.165);
#1683=VECTOR('',#5648,0.164999999999999);
#1684=VECTOR('',#5655,0.210000000000001);
#1685=VECTOR('',#5662,0.21);
#1686=VECTOR('',#5669,0.21);
#1687=VECTOR('',#5676,0.210000000000001);
#1688=VECTOR('',#5683,0.274999999999999);
#1689=VECTOR('',#5690,0.275);
#1690=VECTOR('',#5697,0.275);
#1691=VECTOR('',#5704,0.274999999999999);
#1692=VECTOR('',#5711,0.164999999999999);
#1693=VECTOR('',#5718,0.164999999999999);
#1694=VECTOR('',#5725,0.165);
#1695=VECTOR('',#5732,0.164999999999999);
#1696=VECTOR('',#5737,1.);
#1697=VECTOR('',#5738,1.);
#1698=VECTOR('',#5739,1.);
#1699=VECTOR('',#5740,1.);
#1700=VECTOR('',#5743,1.);
#1701=VECTOR('',#5744,1.);
#1702=VECTOR('',#5745,1.);
#1703=VECTOR('',#5748,1.);
#1704=VECTOR('',#5749,1.);
#1705=VECTOR('',#5750,1.);
#1706=VECTOR('',#5753,1.);
#1707=VECTOR('',#5754,1.);
#1708=VECTOR('',#5763,1.);
#1709=VECTOR('',#5764,1.);
#1710=VECTOR('',#5765,1.);
#1711=VECTOR('',#5766,1.);
#1712=VECTOR('',#5769,1.);
#1713=VECTOR('',#5770,1.);
#1714=VECTOR('',#5771,1.);
#1715=VECTOR('',#5774,1.);
#1716=VECTOR('',#5775,1.);
#1717=VECTOR('',#5776,1.);
#1718=VECTOR('',#5779,1.);
#1719=VECTOR('',#5780,1.);
#1720=VECTOR('',#5781,1.);
#1721=VECTOR('',#5784,1.);
#1722=VECTOR('',#5785,1.);
#1723=VECTOR('',#5786,1.);
#1724=VECTOR('',#5789,1.);
#1725=VECTOR('',#5790,1.);
#1726=VECTOR('',#5791,1.);
#1727=VECTOR('',#5794,1.);
#1728=VECTOR('',#5795,1.);
#1729=VECTOR('',#5796,1.);
#1730=VECTOR('',#5799,1.);
#1731=VECTOR('',#5800,1.);
#1732=VECTOR('',#5801,1.);
#1733=VECTOR('',#5804,1.);
#1734=VECTOR('',#5805,1.);
#1735=VECTOR('',#5806,1.);
#1736=VECTOR('',#5809,1.);
#1737=VECTOR('',#5810,1.);
#1738=VECTOR('',#5811,1.);
#1739=VECTOR('',#5812,1.);
#1740=VECTOR('',#5815,1.);
#1741=VECTOR('',#5816,1.);
#1742=VECTOR('',#5817,1.);
#1743=VECTOR('',#5820,1.);
#1744=VECTOR('',#5821,1.);
#1745=VECTOR('',#5822,1.);
#1746=VECTOR('',#5825,1.);
#1747=VECTOR('',#5826,1.);
#1748=VECTOR('',#5827,1.);
#1749=VECTOR('',#5830,1.);
#1750=VECTOR('',#5831,1.);
#1751=VECTOR('',#5832,1.);
#1752=VECTOR('',#5835,1.);
#1753=VECTOR('',#5836,1.);
#1754=VECTOR('',#5837,1.);
#1755=VECTOR('',#5840,1.);
#1756=VECTOR('',#5841,1.);
#1757=VECTOR('',#5842,1.);
#1758=VECTOR('',#5845,1.);
#1759=VECTOR('',#5846,1.);
#1760=VECTOR('',#5847,1.);
#1761=VECTOR('',#5850,1.);
#1762=VECTOR('',#5851,1.);
#1763=VECTOR('',#5852,1.);
#1764=VECTOR('',#5855,1.);
#1765=VECTOR('',#5856,1.);
#1766=VECTOR('',#5857,1.);
#1767=VECTOR('',#5858,1.);
#1768=VECTOR('',#5861,1.);
#1769=VECTOR('',#5862,1.);
#1770=VECTOR('',#5863,1.);
#1771=VECTOR('',#5866,1.);
#1772=VECTOR('',#5867,1.);
#1773=VECTOR('',#5868,1.);
#1774=VECTOR('',#5871,1.);
#1775=VECTOR('',#5872,1.);
#1776=VECTOR('',#5873,1.);
#1777=VECTOR('',#5876,1.);
#1778=VECTOR('',#5877,1.);
#1779=VECTOR('',#5878,1.);
#1780=VECTOR('',#5881,1.);
#1781=VECTOR('',#5882,1.);
#1782=VECTOR('',#5883,1.);
#1783=VECTOR('',#5886,1.);
#1784=VECTOR('',#5887,1.);
#1785=VECTOR('',#5888,1.);
#1786=VECTOR('',#5891,1.);
#1787=VECTOR('',#5892,1.);
#1788=VECTOR('',#5893,1.);
#1789=VECTOR('',#5896,1.);
#1790=VECTOR('',#5897,1.);
#1791=VECTOR('',#5898,1.);
#1792=VECTOR('',#5901,1.);
#1793=VECTOR('',#5902,1.);
#1794=VECTOR('',#5903,1.);
#1795=VECTOR('',#5904,1.);
#1796=VECTOR('',#5907,1.);
#1797=VECTOR('',#5908,1.);
#1798=VECTOR('',#5909,1.);
#1799=VECTOR('',#5912,1.);
#1800=VECTOR('',#5913,1.);
#1801=VECTOR('',#5914,1.);
#1802=VECTOR('',#5917,1.);
#1803=VECTOR('',#5918,1.);
#1804=VECTOR('',#5919,1.);
#1805=VECTOR('',#5922,1.);
#1806=VECTOR('',#5923,1.);
#1807=VECTOR('',#5924,1.);
#1808=VECTOR('',#5927,1.);
#1809=VECTOR('',#5928,1.);
#1810=VECTOR('',#5929,1.);
#1811=VECTOR('',#5932,1.);
#1812=VECTOR('',#5933,1.);
#1813=VECTOR('',#5934,1.);
#1814=VECTOR('',#5937,1.);
#1815=VECTOR('',#5938,1.);
#1816=VECTOR('',#5939,1.);
#1817=VECTOR('',#5942,1.);
#1818=VECTOR('',#5943,1.);
#1819=VECTOR('',#5944,1.);
#1820=VECTOR('',#5949,0.21);
#1821=VECTOR('',#5954,1.);
#1822=VECTOR('',#5955,1.);
#1823=VECTOR('',#5956,1.);
#1824=VECTOR('',#5959,1.);
#1825=VECTOR('',#5960,1.);
#1826=VECTOR('',#5961,1.);
#1827=VECTOR('',#5964,1.);
#1828=VECTOR('',#5965,1.);
#1829=VECTOR('',#5968,1.);
#1830=VECTOR('',#5969,1.);
#1831=VECTOR('',#5970,1.);
#1832=VECTOR('',#5973,1.);
#1833=VECTOR('',#5974,1.);
#1834=VECTOR('',#5977,1.);
#1835=VECTOR('',#5978,1.);
#1836=VECTOR('',#5979,1.);
#1837=VECTOR('',#5982,1.);
#1838=VECTOR('',#5983,1.);
#1839=VECTOR('',#5986,1.);
#1840=VECTOR('',#5987,1.);
#1841=VECTOR('',#5996,1.);
#1842=VECTOR('',#5997,1.);
#1843=VECTOR('',#5998,1.);
#1844=VECTOR('',#5999,1.);
#1845=VECTOR('',#6002,1.);
#1846=VECTOR('',#6003,1.);
#1847=VECTOR('',#6004,1.);
#1848=VECTOR('',#6007,1.);
#1849=VECTOR('',#6008,1.);
#1850=VECTOR('',#6009,1.);
#1851=VECTOR('',#6014,1.);
#1852=VECTOR('',#6015,1.);
#1853=VECTOR('',#6016,1.);
#1854=VECTOR('',#6017,1.);
#1855=VECTOR('',#6018,1.);
#1856=VECTOR('',#6019,1.);
#1857=VECTOR('',#6020,1.);
#1858=VECTOR('',#6023,1.);
#1859=VECTOR('',#6024,1.);
#1860=VECTOR('',#6027,1.);
#1861=VECTOR('',#6028,1.);
#1862=VECTOR('',#6031,1.);
#1863=VECTOR('',#6032,1.);
#1864=VECTOR('',#6033,1.);
#1865=VECTOR('',#6034,1.);
#1866=VECTOR('',#6035,1.);
#1867=VECTOR('',#6038,1.);
#1868=VECTOR('',#6041,1.);
#1869=VECTOR('',#6044,1.);
#1870=VECTOR('',#6049,0.21);
#1871=VECTOR('',#6058,1.);
#1872=VECTOR('',#6061,1.);
#1873=VECTOR('',#6064,1.);
#1874=VECTOR('',#6071,1.);
#1875=VECTOR('',#6072,1.);
#1876=VECTOR('',#6073,1.);
#1877=VECTOR('',#6074,1.);
#1878=VECTOR('',#6077,1.);
#1879=VECTOR('',#6078,1.);
#1880=VECTOR('',#6079,1.);
#1881=VECTOR('',#6082,1.);
#1882=VECTOR('',#6083,1.);
#1883=VECTOR('',#6084,1.);
#1884=VECTOR('',#6087,1.);
#1885=VECTOR('',#6088,1.);
#1886=VECTOR('',#6089,1.);
#1887=VECTOR('',#6092,1.);
#1888=VECTOR('',#6093,1.);
#1889=VECTOR('',#6094,1.);
#1890=VECTOR('',#6097,1.);
#1891=VECTOR('',#6098,1.);
#1892=VECTOR('',#6115,0.4);
#1893=VECTOR('',#6120,0.425);
#1894=VECTOR('',#6125,0.41);
#1895=VECTOR('',#6134,0.26);
#1896=VECTOR('',#6137,0.25);
#1897=VECTOR('',#6144,0.375);
#1898=VECTOR('',#6155,0.375);
#1899=VECTOR('',#6166,0.375);
#1900=VECTOR('',#6177,0.375);
#1901=VECTOR('',#6188,0.225);
#1902=VECTOR('',#6193,0.225);
#1903=VECTOR('',#6198,0.225);
#1904=VECTOR('',#6203,0.225000000000001);
#1905=VECTOR('',#6206,1.);
#1906=VECTOR('',#6207,1.);
#1907=VECTOR('',#6208,1.);
#1908=VECTOR('',#6209,1.);
#1909=VECTOR('',#6212,1.);
#1910=VECTOR('',#6213,1.);
#1911=VECTOR('',#6214,1.);
#1912=VECTOR('',#6217,1.);
#1913=VECTOR('',#6218,1.);
#1914=VECTOR('',#6219,1.);
#1915=VECTOR('',#6222,1.);
#1916=VECTOR('',#6223,1.);
#1917=VECTOR('',#6224,1.);
#1918=VECTOR('',#6227,1.);
#1919=VECTOR('',#6228,1.);
#1920=VECTOR('',#6229,1.);
#1921=VECTOR('',#6232,1.);
#1922=VECTOR('',#6233,1.);
#1923=VECTOR('',#6234,1.);
#1924=VECTOR('',#6237,1.);
#1925=VECTOR('',#6238,1.);
#1926=VECTOR('',#6239,1.);
#1927=VECTOR('',#6242,1.);
#1928=VECTOR('',#6243,1.);
#1929=VECTOR('',#6244,1.);
#1930=VECTOR('',#6247,1.);
#1931=VECTOR('',#6248,1.);
#1932=VECTOR('',#6249,1.);
#1933=VECTOR('',#6252,1.);
#1934=VECTOR('',#6253,1.);
#1935=VECTOR('',#6254,1.);
#1936=VECTOR('',#6257,1.);
#1937=VECTOR('',#6258,1.);
#1938=VECTOR('',#6259,1.);
#1939=VECTOR('',#6262,1.);
#1940=VECTOR('',#6263,1.);
#1941=VECTOR('',#6278,0.325);
#1942=VECTOR('',#6283,0.35);
#1943=VECTOR('',#6288,0.335);
#1944=VECTOR('',#6297,0.21);
#1945=VECTOR('',#6302,0.2);
#1946=VECTOR('',#6307,0.18);
#1947=VECTOR('',#6312,1.);
#1948=VECTOR('',#6313,1.);
#1949=VECTOR('',#6314,1.);
#1950=VECTOR('',#6315,1.);
#1951=VECTOR('',#6318,1.);
#1952=VECTOR('',#6319,1.);
#1953=VECTOR('',#6320,1.);
#1954=VECTOR('',#6323,1.);
#1955=VECTOR('',#6324,1.);
#1956=VECTOR('',#6325,1.);
#1957=VECTOR('',#6328,1.);
#1958=VECTOR('',#6329,1.);
#1959=VECTOR('',#6330,1.);
#1960=VECTOR('',#6333,1.);
#1961=VECTOR('',#6334,1.);
#1962=VECTOR('',#6335,1.);
#1963=VECTOR('',#6338,1.);
#1964=VECTOR('',#6339,1.);
#1965=VECTOR('',#6350,0.475);
#1966=VECTOR('',#6361,0.475);
#1967=VECTOR('',#6372,0.275);
#1968=VECTOR('',#6377,0.275);
#1969=VECTOR('',#6380,1.);
#1970=VECTOR('',#6381,1.);
#1971=VECTOR('',#6382,1.);
#1972=VECTOR('',#6383,1.);
#1973=VECTOR('',#6386,1.);
#1974=VECTOR('',#6387,1.);
#1975=VECTOR('',#6388,1.);
#1976=VECTOR('',#6391,1.);
#1977=VECTOR('',#6392,1.);
#1978=VECTOR('',#6393,1.);
#1979=VECTOR('',#6396,1.);
#1980=VECTOR('',#6397,1.);
#1981=VECTOR('',#6406,1.);
#1982=VECTOR('',#6407,1.);
#1983=VECTOR('',#6408,1.);
#1984=VECTOR('',#6409,1.);
#1985=VECTOR('',#6412,1.);
#1986=VECTOR('',#6413,1.);
#1987=VECTOR('',#6414,1.);
#1988=VECTOR('',#6417,1.);
#1989=VECTOR('',#6418,1.);
#1990=VECTOR('',#6419,1.);
#1991=VECTOR('',#6422,1.);
#1992=VECTOR('',#6423,1.);
#1993=VECTOR('',#6432,1.);
#1994=VECTOR('',#6433,1.);
#1995=VECTOR('',#6434,1.);
#1996=VECTOR('',#6435,1.);
#1997=VECTOR('',#6438,1.);
#1998=VECTOR('',#6439,1.);
#1999=VECTOR('',#6440,1.);
#2000=VECTOR('',#6443,1.);
#2001=VECTOR('',#6444,1.);
#2002=VECTOR('',#6445,1.);
#2003=VECTOR('',#6448,1.);
#2004=VECTOR('',#6449,1.);
#2005=VECTOR('',#6462,1.);
#2006=VECTOR('',#6467,1.);
#2007=VECTOR('',#6470,0.21);
#2008=VECTOR('',#6475,1.);
#2009=VECTOR('',#6478,1.);
#2010=VECTOR('',#6483,1.);
#2011=VECTOR('',#6486,0.21);
#2012=VECTOR('',#6491,1.);
#2013=VECTOR('',#6494,1.);
#2014=VECTOR('',#6499,1.);
#2015=VECTOR('',#6502,0.21);
#2016=VECTOR('',#6507,1.);
#2017=VECTOR('',#6510,1.);
#2018=VECTOR('',#6515,1.);
#2019=VECTOR('',#6518,0.21);
#2020=VECTOR('',#6523,1.);
#2021=VECTOR('',#6526,1.);
#2022=VECTOR('',#6527,1.);
#2023=VECTOR('',#6528,1.);
#2024=VECTOR('',#6529,1.);
#2025=VECTOR('',#6530,1.);
#2026=VECTOR('',#6531,1.);
#2027=VECTOR('',#6534,1.);
#2028=VECTOR('',#6535,1.);
#2029=VECTOR('',#6536,1.);
#2030=VECTOR('',#6537,1.);
#2031=VECTOR('',#6538,1.);
#2032=VECTOR('',#6539,1.);
#2033=VECTOR('',#6542,1.);
#2034=VECTOR('',#6543,1.);
#2035=VECTOR('',#6544,1.);
#2036=VECTOR('',#6545,1.);
#2037=VECTOR('',#6546,1.);
#2038=VECTOR('',#6547,1.);
#2039=VECTOR('',#6548,1.);
#2040=VECTOR('',#6549,1.);
#2041=VECTOR('',#6550,1.);
#2042=VECTOR('',#6551,1.);
#2043=VECTOR('',#6554,1.);
#2044=VECTOR('',#6555,1.);
#2045=VECTOR('',#6558,1.);
#2046=VECTOR('',#6559,1.);
#2047=VECTOR('',#6562,1.);
#2048=VECTOR('',#6563,1.);
#2049=VECTOR('',#6566,1.);
#2050=VECTOR('',#6567,1.);
#2051=VECTOR('',#6570,1.);
#2052=VECTOR('',#6573,1.);
#2053=VECTOR('',#6574,1.);
#2054=VECTOR('',#6577,1.);
#2055=VECTOR('',#6578,1.);
#2056=VECTOR('',#6581,1.);
#2057=VECTOR('',#6582,1.);
#2058=VECTOR('',#6585,1.);
#2059=VECTOR('',#6586,1.);
#2060=VECTOR('',#6589,1.);
#2061=VECTOR('',#6596,1.);
#2062=VECTOR('',#6597,1.);
#2063=VECTOR('',#6598,1.);
#2064=VECTOR('',#6599,1.);
#2065=VECTOR('',#6602,1.);
#2066=VECTOR('',#6603,1.);
#2067=VECTOR('',#6604,1.);
#2068=VECTOR('',#6607,1.);
#2069=VECTOR('',#6608,1.);
#2070=VECTOR('',#6609,1.);
#2071=VECTOR('',#6612,1.);
#2072=VECTOR('',#6613,1.);
#2073=VECTOR('',#6614,1.);
#2074=VECTOR('',#6617,1.);
#2075=VECTOR('',#6618,1.);
#2076=VECTOR('',#6619,1.);
#2077=VECTOR('',#6622,1.);
#2078=VECTOR('',#6623,1.);
#2079=VECTOR('',#6624,1.);
#2080=VECTOR('',#6627,1.);
#2081=VECTOR('',#6628,1.);
#2082=VECTOR('',#6629,1.);
#2083=VECTOR('',#6632,1.);
#2084=VECTOR('',#6633,1.);
#2085=VECTOR('',#6642,1.);
#2086=VECTOR('',#6643,1.);
#2087=VECTOR('',#6644,1.);
#2088=VECTOR('',#6645,1.);
#2089=VECTOR('',#6648,1.);
#2090=VECTOR('',#6649,1.);
#2091=VECTOR('',#6650,1.);
#2092=VECTOR('',#6653,1.);
#2093=VECTOR('',#6654,1.);
#2094=VECTOR('',#6655,1.);
#2095=VECTOR('',#6658,1.);
#2096=VECTOR('',#6659,1.);
#2097=VECTOR('',#6660,1.);
#2098=VECTOR('',#6663,1.);
#2099=VECTOR('',#6664,1.);
#2100=VECTOR('',#6665,1.);
#2101=VECTOR('',#6668,1.);
#2102=VECTOR('',#6669,1.);
#2103=VECTOR('',#6670,1.);
#2104=VECTOR('',#6673,1.);
#2105=VECTOR('',#6674,1.);
#2106=VECTOR('',#6675,1.);
#2107=VECTOR('',#6678,1.);
#2108=VECTOR('',#6679,1.);
#2109=VECTOR('',#6696,0.164999999999999);
#2110=VECTOR('',#6703,0.25);
#2111=VECTOR('',#6710,0.275);
#2112=VECTOR('',#6717,0.275);
#2113=VECTOR('',#6724,0.275);
#2114=VECTOR('',#6731,0.275);
#2115=VECTOR('',#6736,1.);
#2116=VECTOR('',#6737,1.);
#2117=VECTOR('',#6738,1.);
#2118=VECTOR('',#6739,1.);
#2119=VECTOR('',#6742,1.);
#2120=VECTOR('',#6743,1.);
#2121=VECTOR('',#6744,1.);
#2122=VECTOR('',#6747,1.);
#2123=VECTOR('',#6748,1.);
#2124=VECTOR('',#6749,1.);
#2125=VECTOR('',#6752,1.);
#2126=VECTOR('',#6753,1.);
#2127=VECTOR('',#6764,0.33);
#2128=VECTOR('',#6771,1.5);
#2129=VECTOR('',#6784,0.275);
#2130=VECTOR('',#6789,0.265);
#2131=VECTOR('',#6798,0.5);
#2132=VECTOR('',#6813,0.4);
#2133=VECTOR('',#6818,0.425);
#2134=VECTOR('',#6823,0.41);
#2135=VECTOR('',#6832,0.26);
#2136=VECTOR('',#6837,0.25);
#2137=VECTOR('',#6842,0.225);
#2138=VECTOR('',#6847,1.);
#2139=VECTOR('',#6848,1.);
#2140=VECTOR('',#6849,1.);
#2141=VECTOR('',#6850,1.);
#2142=VECTOR('',#6853,1.);
#2143=VECTOR('',#6854,1.);
#2144=VECTOR('',#6855,1.);
#2145=VECTOR('',#6858,1.);
#2146=VECTOR('',#6859,1.);
#2147=VECTOR('',#6860,1.);
#2148=VECTOR('',#6863,1.);
#2149=VECTOR('',#6864,1.);
#2150=VECTOR('',#6865,1.);
#2151=VECTOR('',#6868,1.);
#2152=VECTOR('',#6869,1.);
#2153=VECTOR('',#6870,1.);
#2154=VECTOR('',#6873,1.);
#2155=VECTOR('',#6874,1.);
#2156=VECTOR('',#6949,0.32);
#2157=VECTOR('',#6956,0.6);
#2158=VECTOR('',#6973,0.475);
#2159=VECTOR('',#6978,0.5);
#2160=VECTOR('',#6983,0.485);
#2161=VECTOR('',#6992,0.31);
#2162=VECTOR('',#6997,0.3);
#2163=VECTOR('',#7002,0.27);
#2164=VECTOR('',#7007,1.);
#2165=VECTOR('',#7008,1.);
#2166=VECTOR('',#7009,1.);
#2167=VECTOR('',#7010,1.);
#2168=VECTOR('',#7013,1.);
#2169=VECTOR('',#7014,1.);
#2170=VECTOR('',#7015,1.);
#2171=VECTOR('',#7018,1.);
#2172=VECTOR('',#7019,1.);
#2173=VECTOR('',#7020,1.);
#2174=VECTOR('',#7023,1.);
#2175=VECTOR('',#7024,1.);
#2176=VECTOR('',#7025,1.);
#2177=VECTOR('',#7028,1.);
#2178=VECTOR('',#7029,1.);
#2179=VECTOR('',#7030,1.);
#2180=VECTOR('',#7033,1.);
#2181=VECTOR('',#7034,1.);
#2182=CIRCLE('',#5166,0.165);
#2183=CIRCLE('',#5167,0.165);
#2184=CIRCLE('',#5169,0.164999999999999);
#2185=CIRCLE('',#5170,0.164999999999999);
#2186=CIRCLE('',#5172,0.210000000000001);
#2187=CIRCLE('',#5173,0.210000000000001);
#2188=CIRCLE('',#5175,0.21);
#2189=CIRCLE('',#5176,0.21);
#2190=CIRCLE('',#5178,0.21);
#2191=CIRCLE('',#5179,0.21);
#2192=CIRCLE('',#5181,0.210000000000001);
#2193=CIRCLE('',#5182,0.210000000000001);
#2194=CIRCLE('',#5184,0.274999999999999);
#2195=CIRCLE('',#5185,0.274999999999999);
#2196=CIRCLE('',#5187,0.275);
#2197=CIRCLE('',#5188,0.275);
#2198=CIRCLE('',#5190,0.275);
#2199=CIRCLE('',#5191,0.275);
#2200=CIRCLE('',#5193,0.274999999999999);
#2201=CIRCLE('',#5194,0.274999999999999);
#2202=CIRCLE('',#5196,0.164999999999999);
#2203=CIRCLE('',#5197,0.164999999999999);
#2204=CIRCLE('',#5199,0.164999999999999);
#2205=CIRCLE('',#5200,0.164999999999999);
#2206=CIRCLE('',#5202,0.165);
#2207=CIRCLE('',#5203,0.165);
#2208=CIRCLE('',#5205,0.164999999999999);
#2209=CIRCLE('',#5206,0.164999999999999);
#2210=CIRCLE('',#5251,0.21);
#2211=CIRCLE('',#5252,0.21);
#2212=CIRCLE('',#5267,0.2117);
#2213=CIRCLE('',#5276,0.2117);
#2214=CIRCLE('',#5277,0.2117);
#2215=CIRCLE('',#5279,0.2117);
#2216=CIRCLE('',#5294,0.24505);
#2217=CIRCLE('',#5296,0.375);
#2218=CIRCLE('',#5298,0.425);
#2219=CIRCLE('',#5300,0.425);
#2220=CIRCLE('',#5302,0.395);
#2221=CIRCLE('',#5304,0.27);
#2222=CIRCLE('',#5306,0.24505);
#2223=CIRCLE('',#5310,0.375);
#2224=CIRCLE('',#5311,0.375);
#2225=CIRCLE('',#5313,0.225);
#2226=CIRCLE('',#5315,0.375);
#2227=CIRCLE('',#5316,0.375);
#2228=CIRCLE('',#5318,0.225);
#2229=CIRCLE('',#5320,0.375);
#2230=CIRCLE('',#5321,0.375);
#2231=CIRCLE('',#5323,0.225);
#2232=CIRCLE('',#5325,0.375);
#2233=CIRCLE('',#5326,0.375);
#2234=CIRCLE('',#5328,0.225000000000001);
#2235=CIRCLE('',#5330,0.225);
#2236=CIRCLE('',#5332,0.225);
#2237=CIRCLE('',#5334,0.225);
#2238=CIRCLE('',#5336,0.225000000000001);
#2239=CIRCLE('',#5353,0.3);
#2240=CIRCLE('',#5355,0.35);
#2241=CIRCLE('',#5357,0.35);
#2242=CIRCLE('',#5359,0.32);
#2243=CIRCLE('',#5361,0.22);
#2244=CIRCLE('',#5363,0.1954);
#2245=CIRCLE('',#5365,0.1954);
#2246=CIRCLE('',#5367,0.16);
#2247=CIRCLE('',#5379,0.475);
#2248=CIRCLE('',#5380,0.475);
#2249=CIRCLE('',#5382,0.275);
#2250=CIRCLE('',#5384,0.475);
#2251=CIRCLE('',#5385,0.475);
#2252=CIRCLE('',#5387,0.275);
#2253=CIRCLE('',#5389,0.275);
#2254=CIRCLE('',#5391,0.275);
#2255=CIRCLE('',#5416,0.21);
#2256=CIRCLE('',#5418,0.21);
#2257=CIRCLE('',#5419,0.21);
#2258=CIRCLE('',#5420,0.21);
#2259=CIRCLE('',#5422,0.21);
#2260=CIRCLE('',#5424,0.21);
#2261=CIRCLE('',#5425,0.21);
#2262=CIRCLE('',#5426,0.21);
#2263=CIRCLE('',#5428,0.21);
#2264=CIRCLE('',#5430,0.21);
#2265=CIRCLE('',#5431,0.21);
#2266=CIRCLE('',#5432,0.21);
#2267=CIRCLE('',#5434,0.21);
#2268=CIRCLE('',#5436,0.21);
#2269=CIRCLE('',#5437,0.21);
#2270=CIRCLE('',#5438,0.21);
#2271=CIRCLE('',#5480,0.164999999999999);
#2272=CIRCLE('',#5481,0.164999999999999);
#2273=CIRCLE('',#5483,0.25);
#2274=CIRCLE('',#5484,0.25);
#2275=CIRCLE('',#5486,0.275);
#2276=CIRCLE('',#5487,0.275);
#2277=CIRCLE('',#5489,0.275);
#2278=CIRCLE('',#5490,0.275);
#2279=CIRCLE('',#5492,0.275);
#2280=CIRCLE('',#5493,0.275);
#2281=CIRCLE('',#5495,0.275);
#2282=CIRCLE('',#5496,0.275);
#2283=CIRCLE('',#5505,0.33);
#2284=CIRCLE('',#5506,0.33);
#2285=CIRCLE('',#5508,1.5);
#2286=CIRCLE('',#5509,1.5);
#2287=CIRCLE('',#5514,0.285);
#2288=CIRCLE('',#5515,0.265);
#2289=CIRCLE('',#5517,0.265);
#2290=CIRCLE('',#5519,0.5);
#2291=CIRCLE('',#5521,0.5);
#2292=CIRCLE('',#5525,0.375);
#2293=CIRCLE('',#5527,0.425);
#2294=CIRCLE('',#5529,0.425);
#2295=CIRCLE('',#5531,0.395);
#2296=CIRCLE('',#5533,0.27);
#2297=CIRCLE('',#5535,0.24505);
#2298=CIRCLE('',#5537,0.24505);
#2299=CIRCLE('',#5539,0.2);
#2300=CIRCLE('',#5583,0.32);
#2301=CIRCLE('',#5584,0.32);
#2302=CIRCLE('',#5586,0.6);
#2303=CIRCLE('',#5587,0.6);
#2304=CIRCLE('',#5592,0.45);
#2305=CIRCLE('',#5594,0.5);
#2306=CIRCLE('',#5596,0.5);
#2307=CIRCLE('',#5598,0.47);
#2308=CIRCLE('',#5600,0.32);
#2309=CIRCLE('',#5602,0.2942);
#2310=CIRCLE('',#5604,0.2942);
#2311=CIRCLE('',#5606,0.24);
#2312=VERTEX_POINT('',#7073);
#2313=VERTEX_POINT('',#7075);
#2314=VERTEX_POINT('',#7079);
#2315=VERTEX_POINT('',#7081);
#2316=VERTEX_POINT('',#7085);
#2317=VERTEX_POINT('',#7087);
#2318=VERTEX_POINT('',#7091);
#2319=VERTEX_POINT('',#7093);
#2320=VERTEX_POINT('',#7097);
#2321=VERTEX_POINT('',#7099);
#2322=VERTEX_POINT('',#7103);
#2323=VERTEX_POINT('',#7105);
#2324=VERTEX_POINT('',#7109);
#2325=VERTEX_POINT('',#7111);
#2326=VERTEX_POINT('',#7115);
#2327=VERTEX_POINT('',#7117);
#2328=VERTEX_POINT('',#7121);
#2329=VERTEX_POINT('',#7123);
#2330=VERTEX_POINT('',#7127);
#2331=VERTEX_POINT('',#7129);
#2332=VERTEX_POINT('',#7133);
#2333=VERTEX_POINT('',#7135);
#2334=VERTEX_POINT('',#7139);
#2335=VERTEX_POINT('',#7141);
#2336=VERTEX_POINT('',#7145);
#2337=VERTEX_POINT('',#7147);
#2338=VERTEX_POINT('',#7151);
#2339=VERTEX_POINT('',#7153);
#2340=VERTEX_POINT('',#7157);
#2341=VERTEX_POINT('',#7158);
#2342=VERTEX_POINT('',#7160);
#2343=VERTEX_POINT('',#7162);
#2344=VERTEX_POINT('',#7166);
#2345=VERTEX_POINT('',#7168);
#2346=VERTEX_POINT('',#7172);
#2347=VERTEX_POINT('',#7174);
#2348=VERTEX_POINT('',#7184);
#2349=VERTEX_POINT('',#7185);
#2350=VERTEX_POINT('',#7187);
#2351=VERTEX_POINT('',#7189);
#2352=VERTEX_POINT('',#7193);
#2353=VERTEX_POINT('',#7195);
#2354=VERTEX_POINT('',#7199);
#2355=VERTEX_POINT('',#7201);
#2356=VERTEX_POINT('',#7205);
#2357=VERTEX_POINT('',#7207);
#2358=VERTEX_POINT('',#7211);
#2359=VERTEX_POINT('',#7213);
#2360=VERTEX_POINT('',#7217);
#2361=VERTEX_POINT('',#7219);
#2362=VERTEX_POINT('',#7223);
#2363=VERTEX_POINT('',#7225);
#2364=VERTEX_POINT('',#7229);
#2365=VERTEX_POINT('',#7231);
#2366=VERTEX_POINT('',#7235);
#2367=VERTEX_POINT('',#7237);
#2368=VERTEX_POINT('',#7241);
#2369=VERTEX_POINT('',#7242);
#2370=VERTEX_POINT('',#7244);
#2371=VERTEX_POINT('',#7246);
#2372=VERTEX_POINT('',#7250);
#2373=VERTEX_POINT('',#7252);
#2374=VERTEX_POINT('',#7256);
#2375=VERTEX_POINT('',#7258);
#2376=VERTEX_POINT('',#7262);
#2377=VERTEX_POINT('',#7264);
#2378=VERTEX_POINT('',#7268);
#2379=VERTEX_POINT('',#7270);
#2380=VERTEX_POINT('',#7274);
#2381=VERTEX_POINT('',#7276);
#2382=VERTEX_POINT('',#7280);
#2383=VERTEX_POINT('',#7282);
#2384=VERTEX_POINT('',#7286);
#2385=VERTEX_POINT('',#7288);
#2386=VERTEX_POINT('',#7292);
#2387=VERTEX_POINT('',#7294);
#2388=VERTEX_POINT('',#7298);
#2389=VERTEX_POINT('',#7299);
#2390=VERTEX_POINT('',#7301);
#2391=VERTEX_POINT('',#7303);
#2392=VERTEX_POINT('',#7307);
#2393=VERTEX_POINT('',#7309);
#2394=VERTEX_POINT('',#7313);
#2395=VERTEX_POINT('',#7315);
#2396=VERTEX_POINT('',#7319);
#2397=VERTEX_POINT('',#7321);
#2398=VERTEX_POINT('',#7325);
#2399=VERTEX_POINT('',#7327);
#2400=VERTEX_POINT('',#7331);
#2401=VERTEX_POINT('',#7333);
#2402=VERTEX_POINT('',#7337);
#2403=VERTEX_POINT('',#7339);
#2404=VERTEX_POINT('',#7343);
#2405=VERTEX_POINT('',#7345);
#2406=VERTEX_POINT('',#7349);
#2407=VERTEX_POINT('',#7351);
#2408=VERTEX_POINT('',#7355);
#2409=VERTEX_POINT('',#7356);
#2410=VERTEX_POINT('',#7358);
#2411=VERTEX_POINT('',#7360);
#2412=VERTEX_POINT('',#7364);
#2413=VERTEX_POINT('',#7366);
#2414=VERTEX_POINT('',#7370);
#2415=VERTEX_POINT('',#7372);
#2416=VERTEX_POINT('',#7376);
#2417=VERTEX_POINT('',#7378);
#2418=VERTEX_POINT('',#7382);
#2419=VERTEX_POINT('',#7384);
#2420=VERTEX_POINT('',#7388);
#2421=VERTEX_POINT('',#7390);
#2422=VERTEX_POINT('',#7394);
#2423=VERTEX_POINT('',#7396);
#2424=VERTEX_POINT('',#7400);
#2425=VERTEX_POINT('',#7402);
#2426=VERTEX_POINT('',#7406);
#2427=VERTEX_POINT('',#7408);
#2428=VERTEX_POINT('',#7412);
#2429=VERTEX_POINT('',#7414);
#2430=VERTEX_POINT('',#7418);
#2431=VERTEX_POINT('',#7420);
#2432=VERTEX_POINT('',#7424);
#2433=VERTEX_POINT('',#7426);
#2434=VERTEX_POINT('',#7433);
#2435=VERTEX_POINT('',#7435);
#2436=VERTEX_POINT('',#7442);
#2437=VERTEX_POINT('',#7444);
#2438=VERTEX_POINT('',#7457);
#2439=VERTEX_POINT('',#7458);
#2440=VERTEX_POINT('',#7460);
#2441=VERTEX_POINT('',#7462);
#2442=VERTEX_POINT('',#7466);
#2443=VERTEX_POINT('',#7468);
#2444=VERTEX_POINT('',#7472);
#2445=VERTEX_POINT('',#7474);
#2446=VERTEX_POINT('',#7477);
#2447=VERTEX_POINT('',#7480);
#2448=VERTEX_POINT('',#7482);
#2449=VERTEX_POINT('',#7484);
#2450=VERTEX_POINT('',#7486);
#2451=VERTEX_POINT('',#7488);
#2452=VERTEX_POINT('',#7490);
#2453=VERTEX_POINT('',#7494);
#2454=VERTEX_POINT('',#7498);
#2455=VERTEX_POINT('',#7502);
#2456=VERTEX_POINT('',#7504);
#2457=VERTEX_POINT('',#7506);
#2458=VERTEX_POINT('',#7508);
#2459=VERTEX_POINT('',#7514);
#2460=VERTEX_POINT('',#7516);
#2461=VERTEX_POINT('',#7520);
#2462=VERTEX_POINT('',#7523);
#2463=VERTEX_POINT('',#7525);
#2464=VERTEX_POINT('',#7537);
#2465=VERTEX_POINT('',#7538);
#2466=VERTEX_POINT('',#7540);
#2467=VERTEX_POINT('',#7542);
#2468=VERTEX_POINT('',#7546);
#2469=VERTEX_POINT('',#7548);
#2470=VERTEX_POINT('',#7552);
#2471=VERTEX_POINT('',#7554);
#2472=VERTEX_POINT('',#7558);
#2473=VERTEX_POINT('',#7560);
#2474=VERTEX_POINT('',#7564);
#2475=VERTEX_POINT('',#7566);
#2476=VERTEX_POINT('',#7575);
#2477=VERTEX_POINT('',#7578);
#2478=VERTEX_POINT('',#7581);
#2479=VERTEX_POINT('',#7585);
#2480=VERTEX_POINT('',#7589);
#2481=VERTEX_POINT('',#7593);
#2482=VERTEX_POINT('',#7596);
#2483=VERTEX_POINT('',#7603);
#2484=VERTEX_POINT('',#7605);
#2485=VERTEX_POINT('',#7609);
#2486=VERTEX_POINT('',#7612);
#2487=VERTEX_POINT('',#7614);
#2488=VERTEX_POINT('',#7618);
#2489=VERTEX_POINT('',#7621);
#2490=VERTEX_POINT('',#7623);
#2491=VERTEX_POINT('',#7627);
#2492=VERTEX_POINT('',#7630);
#2493=VERTEX_POINT('',#7632);
#2494=VERTEX_POINT('',#7636);
#2495=VERTEX_POINT('',#7639);
#2496=VERTEX_POINT('',#7643);
#2497=VERTEX_POINT('',#7647);
#2498=VERTEX_POINT('',#7651);
#2499=VERTEX_POINT('',#7655);
#2500=VERTEX_POINT('',#7656);
#2501=VERTEX_POINT('',#7658);
#2502=VERTEX_POINT('',#7660);
#2503=VERTEX_POINT('',#7664);
#2504=VERTEX_POINT('',#7666);
#2505=VERTEX_POINT('',#7670);
#2506=VERTEX_POINT('',#7672);
#2507=VERTEX_POINT('',#7676);
#2508=VERTEX_POINT('',#7678);
#2509=VERTEX_POINT('',#7682);
#2510=VERTEX_POINT('',#7684);
#2511=VERTEX_POINT('',#7688);
#2512=VERTEX_POINT('',#7690);
#2513=VERTEX_POINT('',#7694);
#2514=VERTEX_POINT('',#7696);
#2515=VERTEX_POINT('',#7700);
#2516=VERTEX_POINT('',#7702);
#2517=VERTEX_POINT('',#7706);
#2518=VERTEX_POINT('',#7708);
#2519=VERTEX_POINT('',#7712);
#2520=VERTEX_POINT('',#7714);
#2521=VERTEX_POINT('',#7718);
#2522=VERTEX_POINT('',#7720);
#2523=VERTEX_POINT('',#7730);
#2524=VERTEX_POINT('',#7733);
#2525=VERTEX_POINT('',#7737);
#2526=VERTEX_POINT('',#7741);
#2527=VERTEX_POINT('',#7745);
#2528=VERTEX_POINT('',#7748);
#2529=VERTEX_POINT('',#7752);
#2530=VERTEX_POINT('',#7756);
#2531=VERTEX_POINT('',#7761);
#2532=VERTEX_POINT('',#7762);
#2533=VERTEX_POINT('',#7764);
#2534=VERTEX_POINT('',#7766);
#2535=VERTEX_POINT('',#7770);
#2536=VERTEX_POINT('',#7772);
#2537=VERTEX_POINT('',#7776);
#2538=VERTEX_POINT('',#7778);
#2539=VERTEX_POINT('',#7782);
#2540=VERTEX_POINT('',#7784);
#2541=VERTEX_POINT('',#7788);
#2542=VERTEX_POINT('',#7790);
#2543=VERTEX_POINT('',#7800);
#2544=VERTEX_POINT('',#7802);
#2545=VERTEX_POINT('',#7806);
#2546=VERTEX_POINT('',#7809);
#2547=VERTEX_POINT('',#7811);
#2548=VERTEX_POINT('',#7815);
#2549=VERTEX_POINT('',#7818);
#2550=VERTEX_POINT('',#7822);
#2551=VERTEX_POINT('',#7826);
#2552=VERTEX_POINT('',#7827);
#2553=VERTEX_POINT('',#7829);
#2554=VERTEX_POINT('',#7831);
#2555=VERTEX_POINT('',#7835);
#2556=VERTEX_POINT('',#7837);
#2557=VERTEX_POINT('',#7841);
#2558=VERTEX_POINT('',#7843);
#2559=VERTEX_POINT('',#7853);
#2560=VERTEX_POINT('',#7854);
#2561=VERTEX_POINT('',#7856);
#2562=VERTEX_POINT('',#7858);
#2563=VERTEX_POINT('',#7862);
#2564=VERTEX_POINT('',#7864);
#2565=VERTEX_POINT('',#7868);
#2566=VERTEX_POINT('',#7870);
#2567=VERTEX_POINT('',#7880);
#2568=VERTEX_POINT('',#7881);
#2569=VERTEX_POINT('',#7883);
#2570=VERTEX_POINT('',#7885);
#2571=VERTEX_POINT('',#7889);
#2572=VERTEX_POINT('',#7891);
#2573=VERTEX_POINT('',#7895);
#2574=VERTEX_POINT('',#7897);
#2575=VERTEX_POINT('',#7909);
#2576=VERTEX_POINT('',#7910);
#2577=VERTEX_POINT('',#7914);
#2578=VERTEX_POINT('',#7916);
#2579=VERTEX_POINT('',#7918);
#2580=VERTEX_POINT('',#7921);
#2581=VERTEX_POINT('',#7925);
#2582=VERTEX_POINT('',#7926);
#2583=VERTEX_POINT('',#7930);
#2584=VERTEX_POINT('',#7932);
#2585=VERTEX_POINT('',#7934);
#2586=VERTEX_POINT('',#7937);
#2587=VERTEX_POINT('',#7941);
#2588=VERTEX_POINT('',#7942);
#2589=VERTEX_POINT('',#7946);
#2590=VERTEX_POINT('',#7948);
#2591=VERTEX_POINT('',#7950);
#2592=VERTEX_POINT('',#7953);
#2593=VERTEX_POINT('',#7957);
#2594=VERTEX_POINT('',#7958);
#2595=VERTEX_POINT('',#7962);
#2596=VERTEX_POINT('',#7964);
#2597=VERTEX_POINT('',#7966);
#2598=VERTEX_POINT('',#7969);
#2599=VERTEX_POINT('',#7974);
#2600=VERTEX_POINT('',#7976);
#2601=VERTEX_POINT('',#7978);
#2602=VERTEX_POINT('',#7980);
#2603=VERTEX_POINT('',#7985);
#2604=VERTEX_POINT('',#7987);
#2605=VERTEX_POINT('',#7989);
#2606=VERTEX_POINT('',#7991);
#2607=VERTEX_POINT('',#7995);
#2608=VERTEX_POINT('',#7997);
#2609=VERTEX_POINT('',#7999);
#2610=VERTEX_POINT('',#8001);
#2611=VERTEX_POINT('',#8004);
#2612=VERTEX_POINT('',#8006);
#2613=VERTEX_POINT('',#8008);
#2614=VERTEX_POINT('',#8010);
#2615=VERTEX_POINT('',#8014);
#2616=VERTEX_POINT('',#8018);
#2617=VERTEX_POINT('',#8022);
#2618=VERTEX_POINT('',#8026);
#2619=VERTEX_POINT('',#8032);
#2620=VERTEX_POINT('',#8036);
#2621=VERTEX_POINT('',#8040);
#2622=VERTEX_POINT('',#8044);
#2623=VERTEX_POINT('',#8052);
#2624=VERTEX_POINT('',#8053);
#2625=VERTEX_POINT('',#8055);
#2626=VERTEX_POINT('',#8057);
#2627=VERTEX_POINT('',#8061);
#2628=VERTEX_POINT('',#8063);
#2629=VERTEX_POINT('',#8067);
#2630=VERTEX_POINT('',#8069);
#2631=VERTEX_POINT('',#8073);
#2632=VERTEX_POINT('',#8075);
#2633=VERTEX_POINT('',#8079);
#2634=VERTEX_POINT('',#8081);
#2635=VERTEX_POINT('',#8085);
#2636=VERTEX_POINT('',#8087);
#2637=VERTEX_POINT('',#8091);
#2638=VERTEX_POINT('',#8093);
#2639=VERTEX_POINT('',#8103);
#2640=VERTEX_POINT('',#8104);
#2641=VERTEX_POINT('',#8106);
#2642=VERTEX_POINT('',#8108);
#2643=VERTEX_POINT('',#8112);
#2644=VERTEX_POINT('',#8114);
#2645=VERTEX_POINT('',#8118);
#2646=VERTEX_POINT('',#8120);
#2647=VERTEX_POINT('',#8124);
#2648=VERTEX_POINT('',#8126);
#2649=VERTEX_POINT('',#8130);
#2650=VERTEX_POINT('',#8132);
#2651=VERTEX_POINT('',#8136);
#2652=VERTEX_POINT('',#8138);
#2653=VERTEX_POINT('',#8142);
#2654=VERTEX_POINT('',#8144);
#2655=VERTEX_POINT('',#8157);
#2656=VERTEX_POINT('',#8159);
#2657=VERTEX_POINT('',#8163);
#2658=VERTEX_POINT('',#8165);
#2659=VERTEX_POINT('',#8169);
#2660=VERTEX_POINT('',#8171);
#2661=VERTEX_POINT('',#8175);
#2662=VERTEX_POINT('',#8177);
#2663=VERTEX_POINT('',#8181);
#2664=VERTEX_POINT('',#8183);
#2665=VERTEX_POINT('',#8187);
#2666=VERTEX_POINT('',#8189);
#2667=VERTEX_POINT('',#8193);
#2668=VERTEX_POINT('',#8194);
#2669=VERTEX_POINT('',#8196);
#2670=VERTEX_POINT('',#8198);
#2671=VERTEX_POINT('',#8202);
#2672=VERTEX_POINT('',#8204);
#2673=VERTEX_POINT('',#8208);
#2674=VERTEX_POINT('',#8210);
#2675=VERTEX_POINT('',#8220);
#2676=VERTEX_POINT('',#8222);
#2677=VERTEX_POINT('',#8226);
#2678=VERTEX_POINT('',#8228);
#2679=VERTEX_POINT('',#8235);
#2680=VERTEX_POINT('',#8237);
#2681=VERTEX_POINT('',#8241);
#2682=VERTEX_POINT('',#8245);
#2683=VERTEX_POINT('',#8248);
#2684=VERTEX_POINT('',#8254);
#2685=VERTEX_POINT('',#8257);
#2686=VERTEX_POINT('',#8261);
#2687=VERTEX_POINT('',#8265);
#2688=VERTEX_POINT('',#8269);
#2689=VERTEX_POINT('',#8272);
#2690=VERTEX_POINT('',#8276);
#2691=VERTEX_POINT('',#8280);
#2692=VERTEX_POINT('',#8285);
#2693=VERTEX_POINT('',#8286);
#2694=VERTEX_POINT('',#8288);
#2695=VERTEX_POINT('',#8290);
#2696=VERTEX_POINT('',#8294);
#2697=VERTEX_POINT('',#8296);
#2698=VERTEX_POINT('',#8300);
#2699=VERTEX_POINT('',#8302);
#2700=VERTEX_POINT('',#8306);
#2701=VERTEX_POINT('',#8308);
#2702=VERTEX_POINT('',#8312);
#2703=VERTEX_POINT('',#8314);
#2704=VERTEX_POINT('',#8356);
#2705=VERTEX_POINT('',#8358);
#2706=VERTEX_POINT('',#8362);
#2707=VERTEX_POINT('',#8364);
#2708=VERTEX_POINT('',#8371);
#2709=VERTEX_POINT('',#8374);
#2710=VERTEX_POINT('',#8378);
#2711=VERTEX_POINT('',#8382);
#2712=VERTEX_POINT('',#8386);
#2713=VERTEX_POINT('',#8389);
#2714=VERTEX_POINT('',#8393);
#2715=VERTEX_POINT('',#8397);
#2716=VERTEX_POINT('',#8402);
#2717=VERTEX_POINT('',#8403);
#2718=VERTEX_POINT('',#8405);
#2719=VERTEX_POINT('',#8407);
#2720=VERTEX_POINT('',#8411);
#2721=VERTEX_POINT('',#8413);
#2722=VERTEX_POINT('',#8417);
#2723=VERTEX_POINT('',#8419);
#2724=VERTEX_POINT('',#8423);
#2725=VERTEX_POINT('',#8425);
#2726=VERTEX_POINT('',#8429);
#2727=VERTEX_POINT('',#8431);
#2728=EDGE_CURVE('',#2312,#2312,#2182,.T.);
#2729=EDGE_CURVE('',#2312,#2313,#1182,.T.);
#2730=EDGE_CURVE('',#2313,#2313,#2183,.T.);
#2731=EDGE_CURVE('',#2314,#2314,#2184,.T.);
#2732=EDGE_CURVE('',#2314,#2315,#1183,.T.);
#2733=EDGE_CURVE('',#2315,#2315,#2185,.T.);
#2734=EDGE_CURVE('',#2316,#2316,#2186,.T.);
#2735=EDGE_CURVE('',#2316,#2317,#1184,.T.);
#2736=EDGE_CURVE('',#2317,#2317,#2187,.T.);
#2737=EDGE_CURVE('',#2318,#2318,#2188,.T.);
#2738=EDGE_CURVE('',#2318,#2319,#1185,.T.);
#2739=EDGE_CURVE('',#2319,#2319,#2189,.T.);
#2740=EDGE_CURVE('',#2320,#2320,#2190,.T.);
#2741=EDGE_CURVE('',#2320,#2321,#1186,.T.);
#2742=EDGE_CURVE('',#2321,#2321,#2191,.T.);
#2743=EDGE_CURVE('',#2322,#2322,#2192,.T.);
#2744=EDGE_CURVE('',#2322,#2323,#1187,.T.);
#2745=EDGE_CURVE('',#2323,#2323,#2193,.T.);
#2746=EDGE_CURVE('',#2324,#2324,#2194,.T.);
#2747=EDGE_CURVE('',#2324,#2325,#1188,.T.);
#2748=EDGE_CURVE('',#2325,#2325,#2195,.T.);
#2749=EDGE_CURVE('',#2326,#2326,#2196,.T.);
#2750=EDGE_CURVE('',#2326,#2327,#1189,.T.);
#2751=EDGE_CURVE('',#2327,#2327,#2197,.T.);
#2752=EDGE_CURVE('',#2328,#2328,#2198,.T.);
#2753=EDGE_CURVE('',#2328,#2329,#1190,.T.);
#2754=EDGE_CURVE('',#2329,#2329,#2199,.T.);
#2755=EDGE_CURVE('',#2330,#2330,#2200,.T.);
#2756=EDGE_CURVE('',#2330,#2331,#1191,.T.);
#2757=EDGE_CURVE('',#2331,#2331,#2201,.T.);
#2758=EDGE_CURVE('',#2332,#2332,#2202,.T.);
#2759=EDGE_CURVE('',#2332,#2333,#1192,.T.);
#2760=EDGE_CURVE('',#2333,#2333,#2203,.T.);
#2761=EDGE_CURVE('',#2334,#2334,#2204,.T.);
#2762=EDGE_CURVE('',#2334,#2335,#1193,.T.);
#2763=EDGE_CURVE('',#2335,#2335,#2205,.T.);
#2764=EDGE_CURVE('',#2336,#2336,#2206,.T.);
#2765=EDGE_CURVE('',#2336,#2337,#1194,.T.);
#2766=EDGE_CURVE('',#2337,#2337,#2207,.T.);
#2767=EDGE_CURVE('',#2338,#2338,#2208,.T.);
#2768=EDGE_CURVE('',#2338,#2339,#1195,.T.);
#2769=EDGE_CURVE('',#2339,#2339,#2209,.T.);
#2770=EDGE_CURVE('',#2340,#2341,#1196,.T.);
#2771=EDGE_CURVE('',#2341,#2342,#1197,.T.);
#2772=EDGE_CURVE('',#2343,#2342,#1198,.T.);
#2773=EDGE_CURVE('',#2340,#2343,#1199,.T.);
#2774=EDGE_CURVE('',#2344,#2340,#1200,.T.);
#2775=EDGE_CURVE('',#2345,#2343,#1201,.T.);
#2776=EDGE_CURVE('',#2344,#2345,#1202,.T.);
#2777=EDGE_CURVE('',#2346,#2344,#1203,.T.);
#2778=EDGE_CURVE('',#2347,#2345,#1204,.T.);
#2779=EDGE_CURVE('',#2346,#2347,#1205,.T.);
#2780=EDGE_CURVE('',#2341,#2346,#1206,.T.);
#2781=EDGE_CURVE('',#2342,#2347,#1207,.T.);
#2782=EDGE_CURVE('',#2348,#2349,#1208,.T.);
#2783=EDGE_CURVE('',#2348,#2350,#1209,.T.);
#2784=EDGE_CURVE('',#2351,#2350,#1210,.T.);
#2785=EDGE_CURVE('',#2349,#2351,#1211,.T.);
#2786=EDGE_CURVE('',#2352,#2348,#1212,.T.);
#2787=EDGE_CURVE('',#2352,#2353,#1213,.T.);
#2788=EDGE_CURVE('',#2350,#2353,#1214,.T.);
#2789=EDGE_CURVE('',#2354,#2352,#1215,.T.);
#2790=EDGE_CURVE('',#2354,#2355,#1216,.T.);
#2791=EDGE_CURVE('',#2353,#2355,#1217,.T.);
#2792=EDGE_CURVE('',#2356,#2354,#1218,.T.);
#2793=EDGE_CURVE('',#2356,#2357,#1219,.T.);
#2794=EDGE_CURVE('',#2355,#2357,#1220,.T.);
#2795=EDGE_CURVE('',#2358,#2356,#1221,.T.);
#2796=EDGE_CURVE('',#2358,#2359,#1222,.T.);
#2797=EDGE_CURVE('',#2357,#2359,#1223,.T.);
#2798=EDGE_CURVE('',#2360,#2358,#1224,.T.);
#2799=EDGE_CURVE('',#2360,#2361,#1225,.T.);
#2800=EDGE_CURVE('',#2359,#2361,#1226,.T.);
#2801=EDGE_CURVE('',#2362,#2360,#1227,.T.);
#2802=EDGE_CURVE('',#2362,#2363,#1228,.T.);
#2803=EDGE_CURVE('',#2361,#2363,#1229,.T.);
#2804=EDGE_CURVE('',#2364,#2362,#1230,.T.);
#2805=EDGE_CURVE('',#2364,#2365,#1231,.T.);
#2806=EDGE_CURVE('',#2363,#2365,#1232,.T.);
#2807=EDGE_CURVE('',#2366,#2364,#1233,.T.);
#2808=EDGE_CURVE('',#2367,#2366,#1234,.T.);
#2809=EDGE_CURVE('',#2365,#2367,#1235,.T.);
#2810=EDGE_CURVE('',#2368,#2369,#1236,.T.);
#2811=EDGE_CURVE('',#2368,#2370,#1237,.T.);
#2812=EDGE_CURVE('',#2371,#2370,#1238,.T.);
#2813=EDGE_CURVE('',#2369,#2371,#1239,.T.);
#2814=EDGE_CURVE('',#2372,#2368,#1240,.T.);
#2815=EDGE_CURVE('',#2372,#2373,#1241,.T.);
#2816=EDGE_CURVE('',#2370,#2373,#1242,.T.);
#2817=EDGE_CURVE('',#2374,#2372,#1243,.T.);
#2818=EDGE_CURVE('',#2374,#2375,#1244,.T.);
#2819=EDGE_CURVE('',#2373,#2375,#1245,.T.);
#2820=EDGE_CURVE('',#2376,#2374,#1246,.T.);
#2821=EDGE_CURVE('',#2376,#2377,#1247,.T.);
#2822=EDGE_CURVE('',#2375,#2377,#1248,.T.);
#2823=EDGE_CURVE('',#2378,#2376,#1249,.T.);
#2824=EDGE_CURVE('',#2378,#2379,#1250,.T.);
#2825=EDGE_CURVE('',#2377,#2379,#1251,.T.);
#2826=EDGE_CURVE('',#2380,#2378,#1252,.T.);
#2827=EDGE_CURVE('',#2380,#2381,#1253,.T.);
#2828=EDGE_CURVE('',#2379,#2381,#1254,.T.);
#2829=EDGE_CURVE('',#2382,#2380,#1255,.T.);
#2830=EDGE_CURVE('',#2382,#2383,#1256,.T.);
#2831=EDGE_CURVE('',#2381,#2383,#1257,.T.);
#2832=EDGE_CURVE('',#2384,#2382,#1258,.T.);
#2833=EDGE_CURVE('',#2384,#2385,#1259,.T.);
#2834=EDGE_CURVE('',#2383,#2385,#1260,.T.);
#2835=EDGE_CURVE('',#2386,#2384,#1261,.T.);
#2836=EDGE_CURVE('',#2387,#2386,#1262,.T.);
#2837=EDGE_CURVE('',#2385,#2387,#1263,.T.);
#2838=EDGE_CURVE('',#2388,#2389,#1264,.T.);
#2839=EDGE_CURVE('',#2388,#2390,#1265,.T.);
#2840=EDGE_CURVE('',#2391,#2390,#1266,.T.);
#2841=EDGE_CURVE('',#2389,#2391,#1267,.T.);
#2842=EDGE_CURVE('',#2392,#2388,#1268,.T.);
#2843=EDGE_CURVE('',#2392,#2393,#1269,.T.);
#2844=EDGE_CURVE('',#2390,#2393,#1270,.T.);
#2845=EDGE_CURVE('',#2394,#2392,#1271,.T.);
#2846=EDGE_CURVE('',#2394,#2395,#1272,.T.);
#2847=EDGE_CURVE('',#2393,#2395,#1273,.T.);
#2848=EDGE_CURVE('',#2396,#2394,#1274,.T.);
#2849=EDGE_CURVE('',#2396,#2397,#1275,.T.);
#2850=EDGE_CURVE('',#2395,#2397,#1276,.T.);
#2851=EDGE_CURVE('',#2398,#2396,#1277,.T.);
#2852=EDGE_CURVE('',#2398,#2399,#1278,.T.);
#2853=EDGE_CURVE('',#2397,#2399,#1279,.T.);
#2854=EDGE_CURVE('',#2400,#2398,#1280,.T.);
#2855=EDGE_CURVE('',#2400,#2401,#1281,.T.);
#2856=EDGE_CURVE('',#2399,#2401,#1282,.T.);
#2857=EDGE_CURVE('',#2402,#2400,#1283,.T.);
#2858=EDGE_CURVE('',#2402,#2403,#1284,.T.);
#2859=EDGE_CURVE('',#2401,#2403,#1285,.T.);
#2860=EDGE_CURVE('',#2404,#2402,#1286,.T.);
#2861=EDGE_CURVE('',#2404,#2405,#1287,.T.);
#2862=EDGE_CURVE('',#2403,#2405,#1288,.T.);
#2863=EDGE_CURVE('',#2406,#2404,#1289,.T.);
#2864=EDGE_CURVE('',#2407,#2406,#1290,.T.);
#2865=EDGE_CURVE('',#2405,#2407,#1291,.T.);
#2866=EDGE_CURVE('',#2408,#2409,#1292,.T.);
#2867=EDGE_CURVE('',#2408,#2410,#1293,.T.);
#2868=EDGE_CURVE('',#2411,#2410,#1294,.T.);
#2869=EDGE_CURVE('',#2409,#2411,#1295,.T.);
#2870=EDGE_CURVE('',#2412,#2408,#1296,.T.);
#2871=EDGE_CURVE('',#2412,#2413,#1297,.T.);
#2872=EDGE_CURVE('',#2410,#2413,#1298,.T.);
#2873=EDGE_CURVE('',#2414,#2412,#1299,.T.);
#2874=EDGE_CURVE('',#2414,#2415,#1300,.T.);
#2875=EDGE_CURVE('',#2413,#2415,#1301,.T.);
#2876=EDGE_CURVE('',#2416,#2414,#1302,.T.);
#2877=EDGE_CURVE('',#2416,#2417,#1303,.T.);
#2878=EDGE_CURVE('',#2415,#2417,#1304,.T.);
#2879=EDGE_CURVE('',#2418,#2416,#1305,.T.);
#2880=EDGE_CURVE('',#2418,#2419,#1306,.T.);
#2881=EDGE_CURVE('',#2417,#2419,#1307,.T.);
#2882=EDGE_CURVE('',#2420,#2418,#1308,.T.);
#2883=EDGE_CURVE('',#2420,#2421,#1309,.T.);
#2884=EDGE_CURVE('',#2419,#2421,#1310,.T.);
#2885=EDGE_CURVE('',#2422,#2420,#1311,.T.);
#2886=EDGE_CURVE('',#2422,#2423,#1312,.T.);
#2887=EDGE_CURVE('',#2421,#2423,#1313,.T.);
#2888=EDGE_CURVE('',#2424,#2422,#1314,.T.);
#2889=EDGE_CURVE('',#2424,#2425,#1315,.T.);
#2890=EDGE_CURVE('',#2423,#2425,#1316,.T.);
#2891=EDGE_CURVE('',#2426,#2424,#1317,.T.);
#2892=EDGE_CURVE('',#2427,#2426,#1318,.T.);
#2893=EDGE_CURVE('',#2425,#2427,#1319,.T.);
#2894=EDGE_CURVE('',#2428,#2428,#2210,.T.);
#2895=EDGE_CURVE('',#2428,#2429,#1320,.T.);
#2896=EDGE_CURVE('',#2429,#2429,#2211,.T.);
#2897=EDGE_CURVE('',#2366,#2430,#1321,.T.);
#2898=EDGE_CURVE('',#2430,#2431,#1322,.T.);
#2899=EDGE_CURVE('',#2367,#2431,#1323,.T.);
#2900=EDGE_CURVE('',#2432,#2351,#1324,.T.);
#2901=EDGE_CURVE('',#2433,#2432,#1325,.T.);
#2902=EDGE_CURVE('',#2433,#2349,#1326,.T.);
#2903=EDGE_CURVE('',#2386,#2433,#1327,.T.);
#2904=EDGE_CURVE('',#2387,#2432,#1328,.T.);
#2905=EDGE_CURVE('',#2434,#2371,#1329,.T.);
#2906=EDGE_CURVE('',#2435,#2434,#1330,.T.);
#2907=EDGE_CURVE('',#2435,#2369,#1331,.T.);
#2908=EDGE_CURVE('',#2406,#2435,#1332,.T.);
#2909=EDGE_CURVE('',#2407,#2434,#1333,.T.);
#2910=EDGE_CURVE('',#2436,#2391,#1334,.T.);
#2911=EDGE_CURVE('',#2437,#2436,#1335,.T.);
#2912=EDGE_CURVE('',#2437,#2389,#1336,.T.);
#2913=EDGE_CURVE('',#2426,#2437,#1337,.T.);
#2914=EDGE_CURVE('',#2427,#2436,#1338,.T.);
#2915=EDGE_CURVE('',#2431,#2411,#1339,.T.);
#2916=EDGE_CURVE('',#2430,#2409,#1340,.T.);
#2917=EDGE_CURVE('',#2438,#2439,#1341,.T.);
#2918=EDGE_CURVE('',#2440,#2438,#1342,.T.);
#2919=EDGE_CURVE('',#2441,#2440,#1343,.T.);
#2920=EDGE_CURVE('',#2439,#2441,#1344,.T.);
#2921=EDGE_CURVE('',#2440,#2442,#1345,.T.);
#2922=EDGE_CURVE('',#2443,#2442,#1346,.T.);
#2923=EDGE_CURVE('',#2441,#2443,#1347,.T.);
#2924=EDGE_CURVE('',#2442,#2444,#1348,.T.);
#2925=EDGE_CURVE('',#2444,#2445,#1349,.T.);
#2926=EDGE_CURVE('',#2445,#2443,#1350,.T.);
#2927=EDGE_CURVE('',#2446,#2446,#2212,.T.);
#2928=EDGE_CURVE('',#2447,#2438,#1351,.T.);
#2929=EDGE_CURVE('',#2448,#2447,#1352,.T.);
#2930=EDGE_CURVE('',#2448,#2449,#1353,.T.);
#2931=EDGE_CURVE('',#2450,#2449,#1354,.T.);
#2932=EDGE_CURVE('',#2450,#2451,#1355,.T.);
#2933=EDGE_CURVE('',#2451,#2452,#1356,.T.);
#2934=EDGE_CURVE('',#2452,#2444,#1357,.T.);
#2935=EDGE_CURVE('',#2452,#2453,#1358,.T.);
#2936=EDGE_CURVE('',#2453,#2445,#1359,.T.);
#2937=EDGE_CURVE('',#2454,#2451,#1360,.T.);
#2938=EDGE_CURVE('',#2453,#2454,#1361,.T.);
#2939=EDGE_CURVE('',#2455,#2454,#1362,.T.);
#2940=EDGE_CURVE('',#2456,#2455,#1363,.T.);
#2941=EDGE_CURVE('',#2456,#2457,#1364,.T.);
#2942=EDGE_CURVE('',#2458,#2457,#1365,.T.);
#2943=EDGE_CURVE('',#2458,#2439,#1366,.T.);
#2944=EDGE_CURVE('',#2455,#2450,#1367,.T.);
#2945=EDGE_CURVE('',#2449,#2459,#1368,.T.);
#2946=EDGE_CURVE('',#2459,#2460,#235,.T.);
#2947=EDGE_CURVE('',#2460,#2456,#1369,.T.);
#2948=EDGE_CURVE('',#2461,#2459,#2213,.F.);
#2949=EDGE_CURVE('',#2461,#2446,#1370,.T.);
#2950=EDGE_CURVE('',#2462,#2461,#2214,.F.);
#2951=EDGE_CURVE('',#2463,#2462,#236,.T.);
#2952=EDGE_CURVE('',#2460,#2463,#2215,.F.);
#2953=EDGE_CURVE('',#2462,#2448,#1371,.T.);
#2954=EDGE_CURVE('',#2457,#2463,#1372,.T.);
#2955=EDGE_CURVE('',#2447,#2458,#1373,.T.);
#2956=EDGE_CURVE('',#2464,#2465,#1374,.T.);
#2957=EDGE_CURVE('',#2465,#2466,#1375,.T.);
#2958=EDGE_CURVE('',#2466,#2467,#1376,.T.);
#2959=EDGE_CURVE('',#2464,#2467,#1377,.T.);
#2960=EDGE_CURVE('',#2465,#2468,#1378,.T.);
#2961=EDGE_CURVE('',#2468,#2469,#1379,.T.);
#2962=EDGE_CURVE('',#2469,#2466,#1380,.T.);
#2963=EDGE_CURVE('',#2468,#2470,#1381,.T.);
#2964=EDGE_CURVE('',#2470,#2471,#1382,.T.);
#2965=EDGE_CURVE('',#2471,#2469,#1383,.T.);
#2966=EDGE_CURVE('',#2470,#2472,#1384,.T.);
#2967=EDGE_CURVE('',#2472,#2473,#1385,.T.);
#2968=EDGE_CURVE('',#2473,#2471,#1386,.T.);
#2969=EDGE_CURVE('',#2472,#2474,#1387,.T.);
#2970=EDGE_CURVE('',#2474,#2475,#1388,.T.);
#2971=EDGE_CURVE('',#2475,#2473,#1389,.T.);
#2972=EDGE_CURVE('',#2474,#2464,#1390,.T.);
#2973=EDGE_CURVE('',#2467,#2475,#1391,.T.);
#2974=EDGE_CURVE('',#2476,#2476,#2216,.T.);
#2975=EDGE_CURVE('',#2477,#2477,#2217,.T.);
#2976=EDGE_CURVE('',#2478,#2478,#2218,.T.);
#2977=EDGE_CURVE('',#2478,#2477,#1392,.T.);
#2978=EDGE_CURVE('',#2479,#2479,#2219,.T.);
#2979=EDGE_CURVE('',#2479,#2478,#1393,.T.);
#2980=EDGE_CURVE('',#2480,#2480,#2220,.T.);
#2981=EDGE_CURVE('',#2480,#2479,#1394,.T.);
#2982=EDGE_CURVE('',#2481,#2481,#2221,.T.);
#2983=EDGE_CURVE('',#2482,#2482,#2222,.F.);
#2984=EDGE_CURVE('',#2482,#2481,#1395,.T.);
#2985=EDGE_CURVE('',#2476,#2482,#1396,.T.);
#2986=EDGE_CURVE('',#2483,#2483,#2223,.T.);
#2987=EDGE_CURVE('',#2483,#2484,#1397,.T.);
#2988=EDGE_CURVE('',#2484,#2484,#2224,.T.);
#2989=EDGE_CURVE('',#2485,#2485,#2225,.T.);
#2990=EDGE_CURVE('',#2486,#2486,#2226,.T.);
#2991=EDGE_CURVE('',#2486,#2487,#1398,.T.);
#2992=EDGE_CURVE('',#2487,#2487,#2227,.T.);
#2993=EDGE_CURVE('',#2488,#2488,#2228,.T.);
#2994=EDGE_CURVE('',#2489,#2489,#2229,.T.);
#2995=EDGE_CURVE('',#2489,#2490,#1399,.T.);
#2996=EDGE_CURVE('',#2490,#2490,#2230,.T.);
#2997=EDGE_CURVE('',#2491,#2491,#2231,.T.);
#2998=EDGE_CURVE('',#2492,#2492,#2232,.T.);
#2999=EDGE_CURVE('',#2492,#2493,#1400,.T.);
#3000=EDGE_CURVE('',#2493,#2493,#2233,.T.);
#3001=EDGE_CURVE('',#2494,#2494,#2234,.T.);
#3002=EDGE_CURVE('',#2495,#2495,#2235,.T.);
#3003=EDGE_CURVE('',#2495,#2485,#1401,.T.);
#3004=EDGE_CURVE('',#2496,#2496,#2236,.T.);
#3005=EDGE_CURVE('',#2496,#2488,#1402,.T.);
#3006=EDGE_CURVE('',#2497,#2497,#2237,.T.);
#3007=EDGE_CURVE('',#2497,#2491,#1403,.T.);
#3008=EDGE_CURVE('',#2498,#2498,#2238,.T.);
#3009=EDGE_CURVE('',#2498,#2494,#1404,.T.);
#3010=EDGE_CURVE('',#2499,#2500,#1405,.T.);
#3011=EDGE_CURVE('',#2500,#2501,#1406,.T.);
#3012=EDGE_CURVE('',#2502,#2501,#1407,.T.);
#3013=EDGE_CURVE('',#2499,#2502,#1408,.T.);
#3014=EDGE_CURVE('',#2503,#2499,#1409,.T.);
#3015=EDGE_CURVE('',#2504,#2502,#1410,.T.);
#3016=EDGE_CURVE('',#2503,#2504,#1411,.T.);
#3017=EDGE_CURVE('',#2505,#2503,#1412,.T.);
#3018=EDGE_CURVE('',#2506,#2504,#1413,.T.);
#3019=EDGE_CURVE('',#2505,#2506,#1414,.T.);
#3020=EDGE_CURVE('',#2507,#2505,#1415,.T.);
#3021=EDGE_CURVE('',#2508,#2506,#1416,.T.);
#3022=EDGE_CURVE('',#2507,#2508,#1417,.T.);
#3023=EDGE_CURVE('',#2509,#2507,#1418,.T.);
#3024=EDGE_CURVE('',#2510,#2508,#1419,.T.);
#3025=EDGE_CURVE('',#2509,#2510,#1420,.T.);
#3026=EDGE_CURVE('',#2511,#2509,#1421,.T.);
#3027=EDGE_CURVE('',#2512,#2510,#1422,.T.);
#3028=EDGE_CURVE('',#2511,#2512,#1423,.T.);
#3029=EDGE_CURVE('',#2513,#2511,#1424,.T.);
#3030=EDGE_CURVE('',#2514,#2512,#1425,.T.);
#3031=EDGE_CURVE('',#2513,#2514,#1426,.T.);
#3032=EDGE_CURVE('',#2515,#2513,#1427,.T.);
#3033=EDGE_CURVE('',#2516,#2514,#1428,.T.);
#3034=EDGE_CURVE('',#2515,#2516,#1429,.T.);
#3035=EDGE_CURVE('',#2517,#2515,#1430,.T.);
#3036=EDGE_CURVE('',#2518,#2516,#1431,.T.);
#3037=EDGE_CURVE('',#2517,#2518,#1432,.T.);
#3038=EDGE_CURVE('',#2519,#2517,#1433,.T.);
#3039=EDGE_CURVE('',#2520,#2518,#1434,.T.);
#3040=EDGE_CURVE('',#2519,#2520,#1435,.T.);
#3041=EDGE_CURVE('',#2521,#2519,#1436,.T.);
#3042=EDGE_CURVE('',#2522,#2520,#1437,.T.);
#3043=EDGE_CURVE('',#2521,#2522,#1438,.T.);
#3044=EDGE_CURVE('',#2500,#2521,#1439,.T.);
#3045=EDGE_CURVE('',#2501,#2522,#1440,.T.);
#3046=EDGE_CURVE('',#2523,#2523,#2239,.T.);
#3047=EDGE_CURVE('',#2524,#2524,#2240,.T.);
#3048=EDGE_CURVE('',#2524,#2523,#1441,.T.);
#3049=EDGE_CURVE('',#2525,#2525,#2241,.T.);
#3050=EDGE_CURVE('',#2525,#2524,#1442,.T.);
#3051=EDGE_CURVE('',#2526,#2526,#2242,.T.);
#3052=EDGE_CURVE('',#2526,#2525,#1443,.T.);
#3053=EDGE_CURVE('',#2527,#2527,#2243,.T.);
#3054=EDGE_CURVE('',#2528,#2528,#2244,.F.);
#3055=EDGE_CURVE('',#2528,#2527,#1444,.T.);
#3056=EDGE_CURVE('',#2529,#2529,#2245,.F.);
#3057=EDGE_CURVE('',#2529,#2528,#1445,.T.);
#3058=EDGE_CURVE('',#2530,#2530,#2246,.T.);
#3059=EDGE_CURVE('',#2530,#2529,#1446,.T.);
#3060=EDGE_CURVE('',#2531,#2532,#1447,.T.);
#3061=EDGE_CURVE('',#2532,#2533,#1448,.T.);
#3062=EDGE_CURVE('',#2533,#2534,#1449,.T.);
#3063=EDGE_CURVE('',#2531,#2534,#1450,.T.);
#3064=EDGE_CURVE('',#2532,#2535,#1451,.T.);
#3065=EDGE_CURVE('',#2535,#2536,#1452,.T.);
#3066=EDGE_CURVE('',#2536,#2533,#1453,.T.);
#3067=EDGE_CURVE('',#2535,#2537,#1454,.T.);
#3068=EDGE_CURVE('',#2537,#2538,#1455,.T.);
#3069=EDGE_CURVE('',#2538,#2536,#1456,.T.);
#3070=EDGE_CURVE('',#2537,#2539,#1457,.T.);
#3071=EDGE_CURVE('',#2539,#2540,#1458,.T.);
#3072=EDGE_CURVE('',#2540,#2538,#1459,.T.);
#3073=EDGE_CURVE('',#2539,#2541,#1460,.T.);
#3074=EDGE_CURVE('',#2541,#2542,#1461,.T.);
#3075=EDGE_CURVE('',#2542,#2540,#1462,.T.);
#3076=EDGE_CURVE('',#2541,#2531,#1463,.T.);
#3077=EDGE_CURVE('',#2534,#2542,#1464,.T.);
#3078=EDGE_CURVE('',#2543,#2543,#2247,.T.);
#3079=EDGE_CURVE('',#2543,#2544,#1465,.T.);
#3080=EDGE_CURVE('',#2544,#2544,#2248,.T.);
#3081=EDGE_CURVE('',#2545,#2545,#2249,.T.);
#3082=EDGE_CURVE('',#2546,#2546,#2250,.T.);
#3083=EDGE_CURVE('',#2546,#2547,#1466,.T.);
#3084=EDGE_CURVE('',#2547,#2547,#2251,.T.);
#3085=EDGE_CURVE('',#2548,#2548,#2252,.T.);
#3086=EDGE_CURVE('',#2549,#2549,#2253,.T.);
#3087=EDGE_CURVE('',#2549,#2545,#1467,.T.);
#3088=EDGE_CURVE('',#2550,#2550,#2254,.T.);
#3089=EDGE_CURVE('',#2550,#2548,#1468,.T.);
#3090=EDGE_CURVE('',#2551,#2552,#1469,.T.);
#3091=EDGE_CURVE('',#2552,#2553,#1470,.T.);
#3092=EDGE_CURVE('',#2554,#2553,#1471,.T.);
#3093=EDGE_CURVE('',#2551,#2554,#1472,.T.);
#3094=EDGE_CURVE('',#2555,#2551,#1473,.T.);
#3095=EDGE_CURVE('',#2556,#2554,#1474,.T.);
#3096=EDGE_CURVE('',#2555,#2556,#1475,.T.);
#3097=EDGE_CURVE('',#2557,#2555,#1476,.T.);
#3098=EDGE_CURVE('',#2558,#2556,#1477,.T.);
#3099=EDGE_CURVE('',#2557,#2558,#1478,.T.);
#3100=EDGE_CURVE('',#2552,#2557,#1479,.T.);
#3101=EDGE_CURVE('',#2553,#2558,#1480,.T.);
#3102=EDGE_CURVE('',#2559,#2560,#1481,.T.);
#3103=EDGE_CURVE('',#2560,#2561,#1482,.T.);
#3104=EDGE_CURVE('',#2562,#2561,#1483,.T.);
#3105=EDGE_CURVE('',#2559,#2562,#1484,.T.);
#3106=EDGE_CURVE('',#2563,#2559,#1485,.T.);
#3107=EDGE_CURVE('',#2564,#2562,#1486,.T.);
#3108=EDGE_CURVE('',#2563,#2564,#1487,.T.);
#3109=EDGE_CURVE('',#2565,#2563,#1488,.T.);
#3110=EDGE_CURVE('',#2566,#2564,#1489,.T.);
#3111=EDGE_CURVE('',#2565,#2566,#1490,.T.);
#3112=EDGE_CURVE('',#2560,#2565,#1491,.T.);
#3113=EDGE_CURVE('',#2561,#2566,#1492,.T.);
#3114=EDGE_CURVE('',#2567,#2568,#1493,.T.);
#3115=EDGE_CURVE('',#2568,#2569,#1494,.T.);
#3116=EDGE_CURVE('',#2570,#2569,#1495,.T.);
#3117=EDGE_CURVE('',#2567,#2570,#1496,.T.);
#3118=EDGE_CURVE('',#2571,#2567,#1497,.T.);
#3119=EDGE_CURVE('',#2572,#2570,#1498,.T.);
#3120=EDGE_CURVE('',#2571,#2572,#1499,.T.);
#3121=EDGE_CURVE('',#2573,#2571,#1500,.T.);
#3122=EDGE_CURVE('',#2574,#2572,#1501,.T.);
#3123=EDGE_CURVE('',#2573,#2574,#1502,.T.);
#3124=EDGE_CURVE('',#2568,#2573,#1503,.T.);
#3125=EDGE_CURVE('',#2569,#2574,#1504,.T.);
#3126=EDGE_CURVE('',#2575,#2576,#1505,.T.);
#3127=EDGE_CURVE('',#2575,#2576,#2255,.T.);
#3128=EDGE_CURVE('',#2577,#2575,#1506,.T.);
#3129=EDGE_CURVE('',#2578,#2577,#2256,.T.);
#3130=EDGE_CURVE('',#2578,#2579,#1507,.T.);
#3131=EDGE_CURVE('',#2579,#2579,#2257,.T.);
#3132=EDGE_CURVE('',#2580,#2578,#2258,.T.);
#3133=EDGE_CURVE('',#2576,#2580,#1508,.T.);
#3134=EDGE_CURVE('',#2581,#2582,#1509,.T.);
#3135=EDGE_CURVE('',#2581,#2582,#2259,.T.);
#3136=EDGE_CURVE('',#2583,#2581,#1510,.T.);
#3137=EDGE_CURVE('',#2584,#2583,#2260,.T.);
#3138=EDGE_CURVE('',#2584,#2585,#1511,.T.);
#3139=EDGE_CURVE('',#2585,#2585,#2261,.T.);
#3140=EDGE_CURVE('',#2586,#2584,#2262,.T.);
#3141=EDGE_CURVE('',#2582,#2586,#1512,.T.);
#3142=EDGE_CURVE('',#2587,#2588,#1513,.T.);
#3143=EDGE_CURVE('',#2587,#2588,#2263,.T.);
#3144=EDGE_CURVE('',#2589,#2587,#1514,.T.);
#3145=EDGE_CURVE('',#2590,#2589,#2264,.T.);
#3146=EDGE_CURVE('',#2590,#2591,#1515,.T.);
#3147=EDGE_CURVE('',#2591,#2591,#2265,.T.);
#3148=EDGE_CURVE('',#2592,#2590,#2266,.T.);
#3149=EDGE_CURVE('',#2588,#2592,#1516,.T.);
#3150=EDGE_CURVE('',#2593,#2594,#1517,.T.);
#3151=EDGE_CURVE('',#2593,#2594,#2267,.T.);
#3152=EDGE_CURVE('',#2595,#2593,#1518,.T.);
#3153=EDGE_CURVE('',#2596,#2595,#2268,.T.);
#3154=EDGE_CURVE('',#2596,#2597,#1519,.T.);
#3155=EDGE_CURVE('',#2597,#2597,#2269,.T.);
#3156=EDGE_CURVE('',#2598,#2596,#2270,.T.);
#3157=EDGE_CURVE('',#2594,#2598,#1520,.T.);
#3158=EDGE_CURVE('',#2580,#2589,#1521,.T.);
#3159=EDGE_CURVE('',#2592,#2599,#1522,.T.);
#3160=EDGE_CURVE('',#2600,#2599,#1523,.T.);
#3161=EDGE_CURVE('',#2600,#2601,#1524,.T.);
#3162=EDGE_CURVE('',#2602,#2601,#1525,.T.);
#3163=EDGE_CURVE('',#2602,#2577,#1526,.T.);
#3164=EDGE_CURVE('',#2586,#2595,#1527,.T.);
#3165=EDGE_CURVE('',#2598,#2603,#1528,.T.);
#3166=EDGE_CURVE('',#2604,#2603,#1529,.T.);
#3167=EDGE_CURVE('',#2605,#2604,#1530,.T.);
#3168=EDGE_CURVE('',#2606,#2605,#1531,.T.);
#3169=EDGE_CURVE('',#2606,#2583,#1532,.T.);
#3170=EDGE_CURVE('',#2599,#2607,#1533,.T.);
#3171=EDGE_CURVE('',#2607,#2608,#1534,.T.);
#3172=EDGE_CURVE('',#2608,#2609,#1535,.T.);
#3173=EDGE_CURVE('',#2609,#2610,#1536,.T.);
#3174=EDGE_CURVE('',#2610,#2606,#1537,.T.);
#3175=EDGE_CURVE('',#2605,#2611,#1538,.T.);
#3176=EDGE_CURVE('',#2611,#2612,#1539,.T.);
#3177=EDGE_CURVE('',#2612,#2613,#1540,.T.);
#3178=EDGE_CURVE('',#2613,#2614,#1541,.T.);
#3179=EDGE_CURVE('',#2614,#2600,#1542,.T.);
#3180=EDGE_CURVE('',#2615,#2602,#1543,.T.);
#3181=EDGE_CURVE('',#2607,#2615,#1544,.T.);
#3182=EDGE_CURVE('',#2616,#2615,#1545,.T.);
#3183=EDGE_CURVE('',#2608,#2616,#1546,.T.);
#3184=EDGE_CURVE('',#2617,#2616,#1547,.T.);
#3185=EDGE_CURVE('',#2609,#2617,#1548,.T.);
#3186=EDGE_CURVE('',#2618,#2617,#1549,.T.);
#3187=EDGE_CURVE('',#2610,#2618,#1550,.T.);
#3188=EDGE_CURVE('',#2603,#2618,#1551,.T.);
#3189=EDGE_CURVE('',#2619,#2604,#1552,.T.);
#3190=EDGE_CURVE('',#2611,#2619,#1553,.T.);
#3191=EDGE_CURVE('',#2620,#2619,#1554,.T.);
#3192=EDGE_CURVE('',#2612,#2620,#1555,.T.);
#3193=EDGE_CURVE('',#2621,#2620,#1556,.T.);
#3194=EDGE_CURVE('',#2613,#2621,#1557,.T.);
#3195=EDGE_CURVE('',#2622,#2621,#1558,.T.);
#3196=EDGE_CURVE('',#2614,#2622,#1559,.T.);
#3197=EDGE_CURVE('',#2601,#2622,#1560,.T.);
#3198=EDGE_CURVE('',#2623,#2624,#1561,.T.);
#3199=EDGE_CURVE('',#2624,#2625,#1562,.T.);
#3200=EDGE_CURVE('',#2626,#2625,#1563,.T.);
#3201=EDGE_CURVE('',#2623,#2626,#1564,.T.);
#3202=EDGE_CURVE('',#2627,#2623,#1565,.T.);
#3203=EDGE_CURVE('',#2628,#2626,#1566,.T.);
#3204=EDGE_CURVE('',#2627,#2628,#1567,.T.);
#3205=EDGE_CURVE('',#2629,#2627,#1568,.T.);
#3206=EDGE_CURVE('',#2630,#2628,#1569,.T.);
#3207=EDGE_CURVE('',#2629,#2630,#1570,.T.);
#3208=EDGE_CURVE('',#2631,#2629,#1571,.T.);
#3209=EDGE_CURVE('',#2632,#2630,#1572,.T.);
#3210=EDGE_CURVE('',#2631,#2632,#1573,.T.);
#3211=EDGE_CURVE('',#2633,#2631,#1574,.T.);
#3212=EDGE_CURVE('',#2634,#2632,#1575,.T.);
#3213=EDGE_CURVE('',#2633,#2634,#1576,.T.);
#3214=EDGE_CURVE('',#2635,#2633,#1577,.T.);
#3215=EDGE_CURVE('',#2636,#2634,#1578,.T.);
#3216=EDGE_CURVE('',#2635,#2636,#1579,.T.);
#3217=EDGE_CURVE('',#2637,#2635,#1580,.T.);
#3218=EDGE_CURVE('',#2638,#2636,#1581,.T.);
#3219=EDGE_CURVE('',#2637,#2638,#1582,.T.);
#3220=EDGE_CURVE('',#2624,#2637,#1583,.T.);
#3221=EDGE_CURVE('',#2625,#2638,#1584,.T.);
#3222=EDGE_CURVE('',#2639,#2640,#1585,.T.);
#3223=EDGE_CURVE('',#2639,#2641,#1586,.T.);
#3224=EDGE_CURVE('',#2642,#2641,#1587,.T.);
#3225=EDGE_CURVE('',#2640,#2642,#1588,.T.);
#3226=EDGE_CURVE('',#2640,#2643,#1589,.T.);
#3227=EDGE_CURVE('',#2644,#2642,#1590,.T.);
#3228=EDGE_CURVE('',#2643,#2644,#1591,.T.);
#3229=EDGE_CURVE('',#2643,#2645,#1592,.T.);
#3230=EDGE_CURVE('',#2646,#2644,#1593,.T.);
#3231=EDGE_CURVE('',#2645,#2646,#1594,.T.);
#3232=EDGE_CURVE('',#2645,#2647,#1595,.T.);
#3233=EDGE_CURVE('',#2648,#2646,#1596,.T.);
#3234=EDGE_CURVE('',#2647,#2648,#1597,.T.);
#3235=EDGE_CURVE('',#2647,#2649,#1598,.T.);
#3236=EDGE_CURVE('',#2650,#2648,#1599,.T.);
#3237=EDGE_CURVE('',#2649,#2650,#1600,.T.);
#3238=EDGE_CURVE('',#2649,#2651,#1601,.T.);
#3239=EDGE_CURVE('',#2652,#2650,#1602,.T.);
#3240=EDGE_CURVE('',#2651,#2652,#1603,.T.);
#3241=EDGE_CURVE('',#2651,#2653,#1604,.T.);
#3242=EDGE_CURVE('',#2654,#2652,#1605,.T.);
#3243=EDGE_CURVE('',#2653,#2654,#1606,.T.);
#3244=EDGE_CURVE('',#2653,#2639,#1607,.T.);
#3245=EDGE_CURVE('',#2641,#2654,#1608,.T.);
#3246=EDGE_CURVE('',#2655,#2655,#2271,.T.);
#3247=EDGE_CURVE('',#2655,#2656,#1609,.T.);
#3248=EDGE_CURVE('',#2656,#2656,#2272,.T.);
#3249=EDGE_CURVE('',#2657,#2657,#2273,.T.);
#3250=EDGE_CURVE('',#2657,#2658,#1610,.T.);
#3251=EDGE_CURVE('',#2658,#2658,#2274,.T.);
#3252=EDGE_CURVE('',#2659,#2659,#2275,.T.);
#3253=EDGE_CURVE('',#2659,#2660,#1611,.T.);
#3254=EDGE_CURVE('',#2660,#2660,#2276,.T.);
#3255=EDGE_CURVE('',#2661,#2661,#2277,.T.);
#3256=EDGE_CURVE('',#2661,#2662,#1612,.T.);
#3257=EDGE_CURVE('',#2662,#2662,#2278,.T.);
#3258=EDGE_CURVE('',#2663,#2663,#2279,.T.);
#3259=EDGE_CURVE('',#2663,#2664,#1613,.T.);
#3260=EDGE_CURVE('',#2664,#2664,#2280,.T.);
#3261=EDGE_CURVE('',#2665,#2665,#2281,.T.);
#3262=EDGE_CURVE('',#2665,#2666,#1614,.T.);
#3263=EDGE_CURVE('',#2666,#2666,#2282,.T.);
#3264=EDGE_CURVE('',#2667,#2668,#1615,.T.);
#3265=EDGE_CURVE('',#2668,#2669,#1616,.T.);
#3266=EDGE_CURVE('',#2670,#2669,#1617,.T.);
#3267=EDGE_CURVE('',#2667,#2670,#1618,.T.);
#3268=EDGE_CURVE('',#2671,#2667,#1619,.T.);
#3269=EDGE_CURVE('',#2672,#2670,#1620,.T.);
#3270=EDGE_CURVE('',#2671,#2672,#1621,.T.);
#3271=EDGE_CURVE('',#2673,#2671,#1622,.T.);
#3272=EDGE_CURVE('',#2674,#2672,#1623,.T.);
#3273=EDGE_CURVE('',#2673,#2674,#1624,.T.);
#3274=EDGE_CURVE('',#2668,#2673,#1625,.T.);
#3275=EDGE_CURVE('',#2669,#2674,#1626,.T.);
#3276=EDGE_CURVE('',#2675,#2675,#2283,.T.);
#3277=EDGE_CURVE('',#2675,#2676,#1627,.T.);
#3278=EDGE_CURVE('',#2676,#2676,#2284,.T.);
#3279=EDGE_CURVE('',#2677,#2677,#2285,.T.);
#3280=EDGE_CURVE('',#2677,#2678,#1628,.T.);
#3281=EDGE_CURVE('',#2678,#2678,#2286,.T.);
#3282=EDGE_CURVE('',#2679,#2679,#2287,.T.);
#3283=EDGE_CURVE('',#2679,#2680,#1629,.T.);
#3284=EDGE_CURVE('',#2680,#2680,#2288,.T.);
#3285=EDGE_CURVE('',#2680,#2681,#1630,.T.);
#3286=EDGE_CURVE('',#2681,#2681,#2289,.T.);
#3287=EDGE_CURVE('',#2682,#2682,#2290,.T.);
#3288=EDGE_CURVE('',#2682,#2683,#1631,.T.);
#3289=EDGE_CURVE('',#2683,#2683,#2291,.T.);
#3290=EDGE_CURVE('',#2684,#2684,#2292,.T.);
#3291=EDGE_CURVE('',#2685,#2685,#2293,.T.);
#3292=EDGE_CURVE('',#2685,#2684,#1632,.T.);
#3293=EDGE_CURVE('',#2686,#2686,#2294,.T.);
#3294=EDGE_CURVE('',#2686,#2685,#1633,.T.);
#3295=EDGE_CURVE('',#2687,#2687,#2295,.T.);
#3296=EDGE_CURVE('',#2687,#2686,#1634,.T.);
#3297=EDGE_CURVE('',#2688,#2688,#2296,.T.);
#3298=EDGE_CURVE('',#2689,#2689,#2297,.F.);
#3299=EDGE_CURVE('',#2689,#2688,#1635,.T.);
#3300=EDGE_CURVE('',#2690,#2690,#2298,.F.);
#3301=EDGE_CURVE('',#2690,#2689,#1636,.T.);
#3302=EDGE_CURVE('',#2691,#2691,#2299,.T.);
#3303=EDGE_CURVE('',#2691,#2690,#1637,.T.);
#3304=EDGE_CURVE('',#2692,#2693,#1638,.T.);
#3305=EDGE_CURVE('',#2693,#2694,#1639,.T.);
#3306=EDGE_CURVE('',#2694,#2695,#1640,.T.);
#3307=EDGE_CURVE('',#2692,#2695,#1641,.T.);
#3308=EDGE_CURVE('',#2693,#2696,#1642,.T.);
#3309=EDGE_CURVE('',#2696,#2697,#1643,.T.);
#3310=EDGE_CURVE('',#2697,#2694,#1644,.T.);
#3311=EDGE_CURVE('',#2696,#2698,#1645,.T.);
#3312=EDGE_CURVE('',#2698,#2699,#1646,.T.);
#3313=EDGE_CURVE('',#2699,#2697,#1647,.T.);
#3314=EDGE_CURVE('',#2698,#2700,#1648,.T.);
#3315=EDGE_CURVE('',#2700,#2701,#1649,.T.);
#3316=EDGE_CURVE('',#2701,#2699,#1650,.T.);
#3317=EDGE_CURVE('',#2700,#2702,#1651,.T.);
#3318=EDGE_CURVE('',#2702,#2703,#1652,.T.);
#3319=EDGE_CURVE('',#2703,#2701,#1653,.T.);
#3320=EDGE_CURVE('',#2702,#2692,#1654,.T.);
#3321=EDGE_CURVE('',#2695,#2703,#1655,.T.);
#3322=EDGE_CURVE('',#2704,#2704,#2300,.T.);
#3323=EDGE_CURVE('',#2704,#2705,#1656,.T.);
#3324=EDGE_CURVE('',#2705,#2705,#2301,.T.);
#3325=EDGE_CURVE('',#2706,#2706,#2302,.T.);
#3326=EDGE_CURVE('',#2706,#2707,#1657,.T.);
#3327=EDGE_CURVE('',#2707,#2707,#2303,.T.);
#3328=EDGE_CURVE('',#2708,#2708,#2304,.T.);
#3329=EDGE_CURVE('',#2709,#2709,#2305,.T.);
#3330=EDGE_CURVE('',#2709,#2708,#1658,.T.);
#3331=EDGE_CURVE('',#2710,#2710,#2306,.T.);
#3332=EDGE_CURVE('',#2710,#2709,#1659,.T.);
#3333=EDGE_CURVE('',#2711,#2711,#2307,.T.);
#3334=EDGE_CURVE('',#2711,#2710,#1660,.T.);
#3335=EDGE_CURVE('',#2712,#2712,#2308,.T.);
#3336=EDGE_CURVE('',#2713,#2713,#2309,.F.);
#3337=EDGE_CURVE('',#2713,#2712,#1661,.T.);
#3338=EDGE_CURVE('',#2714,#2714,#2310,.F.);
#3339=EDGE_CURVE('',#2714,#2713,#1662,.T.);
#3340=EDGE_CURVE('',#2715,#2715,#2311,.T.);
#3341=EDGE_CURVE('',#2715,#2714,#1663,.T.);
#3342=EDGE_CURVE('',#2716,#2717,#1664,.T.);
#3343=EDGE_CURVE('',#2717,#2718,#1665,.T.);
#3344=EDGE_CURVE('',#2718,#2719,#1666,.T.);
#3345=EDGE_CURVE('',#2716,#2719,#1667,.T.);
#3346=EDGE_CURVE('',#2717,#2720,#1668,.T.);
#3347=EDGE_CURVE('',#2720,#2721,#1669,.T.);
#3348=EDGE_CURVE('',#2721,#2718,#1670,.T.);
#3349=EDGE_CURVE('',#2720,#2722,#1671,.T.);
#3350=EDGE_CURVE('',#2722,#2723,#1672,.T.);
#3351=EDGE_CURVE('',#2723,#2721,#1673,.T.);
#3352=EDGE_CURVE('',#2722,#2724,#1674,.T.);
#3353=EDGE_CURVE('',#2724,#2725,#1675,.T.);
#3354=EDGE_CURVE('',#2725,#2723,#1676,.T.);
#3355=EDGE_CURVE('',#2724,#2726,#1677,.T.);
#3356=EDGE_CURVE('',#2726,#2727,#1678,.T.);
#3357=EDGE_CURVE('',#2727,#2725,#1679,.T.);
#3358=EDGE_CURVE('',#2726,#2716,#1680,.T.);
#3359=EDGE_CURVE('',#2719,#2727,#1681,.T.);
#3360=ORIENTED_EDGE('',*,*,#2728,.F.);
#3361=ORIENTED_EDGE('',*,*,#2729,.T.);
#3362=ORIENTED_EDGE('',*,*,#2730,.F.);
#3363=ORIENTED_EDGE('',*,*,#2729,.F.);
#3364=ORIENTED_EDGE('',*,*,#2731,.F.);
#3365=ORIENTED_EDGE('',*,*,#2732,.T.);
#3366=ORIENTED_EDGE('',*,*,#2733,.F.);
#3367=ORIENTED_EDGE('',*,*,#2732,.F.);
#3368=ORIENTED_EDGE('',*,*,#2734,.F.);
#3369=ORIENTED_EDGE('',*,*,#2735,.T.);
#3370=ORIENTED_EDGE('',*,*,#2736,.F.);
#3371=ORIENTED_EDGE('',*,*,#2735,.F.);
#3372=ORIENTED_EDGE('',*,*,#2737,.F.);
#3373=ORIENTED_EDGE('',*,*,#2738,.T.);
#3374=ORIENTED_EDGE('',*,*,#2739,.F.);
#3375=ORIENTED_EDGE('',*,*,#2738,.F.);
#3376=ORIENTED_EDGE('',*,*,#2740,.F.);
#3377=ORIENTED_EDGE('',*,*,#2741,.T.);
#3378=ORIENTED_EDGE('',*,*,#2742,.F.);
#3379=ORIENTED_EDGE('',*,*,#2741,.F.);
#3380=ORIENTED_EDGE('',*,*,#2743,.F.);
#3381=ORIENTED_EDGE('',*,*,#2744,.T.);
#3382=ORIENTED_EDGE('',*,*,#2745,.F.);
#3383=ORIENTED_EDGE('',*,*,#2744,.F.);
#3384=ORIENTED_EDGE('',*,*,#2746,.F.);
#3385=ORIENTED_EDGE('',*,*,#2747,.T.);
#3386=ORIENTED_EDGE('',*,*,#2748,.F.);
#3387=ORIENTED_EDGE('',*,*,#2747,.F.);
#3388=ORIENTED_EDGE('',*,*,#2749,.F.);
#3389=ORIENTED_EDGE('',*,*,#2750,.T.);
#3390=ORIENTED_EDGE('',*,*,#2751,.F.);
#3391=ORIENTED_EDGE('',*,*,#2750,.F.);
#3392=ORIENTED_EDGE('',*,*,#2752,.F.);
#3393=ORIENTED_EDGE('',*,*,#2753,.T.);
#3394=ORIENTED_EDGE('',*,*,#2754,.F.);
#3395=ORIENTED_EDGE('',*,*,#2753,.F.);
#3396=ORIENTED_EDGE('',*,*,#2755,.F.);
#3397=ORIENTED_EDGE('',*,*,#2756,.T.);
#3398=ORIENTED_EDGE('',*,*,#2757,.F.);
#3399=ORIENTED_EDGE('',*,*,#2756,.F.);
#3400=ORIENTED_EDGE('',*,*,#2758,.F.);
#3401=ORIENTED_EDGE('',*,*,#2759,.T.);
#3402=ORIENTED_EDGE('',*,*,#2760,.F.);
#3403=ORIENTED_EDGE('',*,*,#2759,.F.);
#3404=ORIENTED_EDGE('',*,*,#2761,.F.);
#3405=ORIENTED_EDGE('',*,*,#2762,.T.);
#3406=ORIENTED_EDGE('',*,*,#2763,.F.);
#3407=ORIENTED_EDGE('',*,*,#2762,.F.);
#3408=ORIENTED_EDGE('',*,*,#2764,.F.);
#3409=ORIENTED_EDGE('',*,*,#2765,.T.);
#3410=ORIENTED_EDGE('',*,*,#2766,.F.);
#3411=ORIENTED_EDGE('',*,*,#2765,.F.);
#3412=ORIENTED_EDGE('',*,*,#2767,.F.);
#3413=ORIENTED_EDGE('',*,*,#2768,.T.);
#3414=ORIENTED_EDGE('',*,*,#2769,.F.);
#3415=ORIENTED_EDGE('',*,*,#2768,.F.);
#3416=ORIENTED_EDGE('',*,*,#2770,.T.);
#3417=ORIENTED_EDGE('',*,*,#2771,.T.);
#3418=ORIENTED_EDGE('',*,*,#2772,.F.);
#3419=ORIENTED_EDGE('',*,*,#2773,.F.);
#3420=ORIENTED_EDGE('',*,*,#2774,.T.);
#3421=ORIENTED_EDGE('',*,*,#2773,.T.);
#3422=ORIENTED_EDGE('',*,*,#2775,.F.);
#3423=ORIENTED_EDGE('',*,*,#2776,.F.);
#3424=ORIENTED_EDGE('',*,*,#2777,.T.);
#3425=ORIENTED_EDGE('',*,*,#2776,.T.);
#3426=ORIENTED_EDGE('',*,*,#2778,.F.);
#3427=ORIENTED_EDGE('',*,*,#2779,.F.);
#3428=ORIENTED_EDGE('',*,*,#2780,.T.);
#3429=ORIENTED_EDGE('',*,*,#2779,.T.);
#3430=ORIENTED_EDGE('',*,*,#2781,.F.);
#3431=ORIENTED_EDGE('',*,*,#2771,.F.);
#3432=ORIENTED_EDGE('',*,*,#2781,.T.);
#3433=ORIENTED_EDGE('',*,*,#2778,.T.);
#3434=ORIENTED_EDGE('',*,*,#2775,.T.);
#3435=ORIENTED_EDGE('',*,*,#2772,.T.);
#3436=ORIENTED_EDGE('',*,*,#2736,.T.);
#3437=ORIENTED_EDGE('',*,*,#2739,.T.);
#3438=ORIENTED_EDGE('',*,*,#2742,.T.);
#3439=ORIENTED_EDGE('',*,*,#2745,.T.);
#3440=ORIENTED_EDGE('',*,*,#2769,.T.);
#3441=ORIENTED_EDGE('',*,*,#2766,.T.);
#3442=ORIENTED_EDGE('',*,*,#2763,.T.);
#3443=ORIENTED_EDGE('',*,*,#2760,.T.);
#3444=ORIENTED_EDGE('',*,*,#2757,.T.);
#3445=ORIENTED_EDGE('',*,*,#2754,.T.);
#3446=ORIENTED_EDGE('',*,*,#2751,.T.);
#3447=ORIENTED_EDGE('',*,*,#2748,.T.);
#3448=ORIENTED_EDGE('',*,*,#2733,.T.);
#3449=ORIENTED_EDGE('',*,*,#2730,.T.);
#3450=ORIENTED_EDGE('',*,*,#2780,.F.);
#3451=ORIENTED_EDGE('',*,*,#2770,.F.);
#3452=ORIENTED_EDGE('',*,*,#2774,.F.);
#3453=ORIENTED_EDGE('',*,*,#2777,.F.);
#3454=ORIENTED_EDGE('',*,*,#2734,.T.);
#3455=ORIENTED_EDGE('',*,*,#2737,.T.);
#3456=ORIENTED_EDGE('',*,*,#2740,.T.);
#3457=ORIENTED_EDGE('',*,*,#2743,.T.);
#3458=ORIENTED_EDGE('',*,*,#2767,.T.);
#3459=ORIENTED_EDGE('',*,*,#2764,.T.);
#3460=ORIENTED_EDGE('',*,*,#2761,.T.);
#3461=ORIENTED_EDGE('',*,*,#2758,.T.);
#3462=ORIENTED_EDGE('',*,*,#2755,.T.);
#3463=ORIENTED_EDGE('',*,*,#2752,.T.);
#3464=ORIENTED_EDGE('',*,*,#2749,.T.);
#3465=ORIENTED_EDGE('',*,*,#2746,.T.);
#3466=ORIENTED_EDGE('',*,*,#2731,.T.);
#3467=ORIENTED_EDGE('',*,*,#2728,.T.);
#3468=ORIENTED_EDGE('',*,*,#2782,.F.);
#3469=ORIENTED_EDGE('',*,*,#2783,.T.);
#3470=ORIENTED_EDGE('',*,*,#2784,.F.);
#3471=ORIENTED_EDGE('',*,*,#2785,.F.);
#3472=ORIENTED_EDGE('',*,*,#2786,.F.);
#3473=ORIENTED_EDGE('',*,*,#2787,.T.);
#3474=ORIENTED_EDGE('',*,*,#2788,.F.);
#3475=ORIENTED_EDGE('',*,*,#2783,.F.);
#3476=ORIENTED_EDGE('',*,*,#2789,.F.);
#3477=ORIENTED_EDGE('',*,*,#2790,.T.);
#3478=ORIENTED_EDGE('',*,*,#2791,.F.);
#3479=ORIENTED_EDGE('',*,*,#2787,.F.);
#3480=ORIENTED_EDGE('',*,*,#2792,.F.);
#3481=ORIENTED_EDGE('',*,*,#2793,.T.);
#3482=ORIENTED_EDGE('',*,*,#2794,.F.);
#3483=ORIENTED_EDGE('',*,*,#2790,.F.);
#3484=ORIENTED_EDGE('',*,*,#2795,.F.);
#3485=ORIENTED_EDGE('',*,*,#2796,.T.);
#3486=ORIENTED_EDGE('',*,*,#2797,.F.);
#3487=ORIENTED_EDGE('',*,*,#2793,.F.);
#3488=ORIENTED_EDGE('',*,*,#2798,.F.);
#3489=ORIENTED_EDGE('',*,*,#2799,.T.);
#3490=ORIENTED_EDGE('',*,*,#2800,.F.);
#3491=ORIENTED_EDGE('',*,*,#2796,.F.);
#3492=ORIENTED_EDGE('',*,*,#2801,.F.);
#3493=ORIENTED_EDGE('',*,*,#2802,.T.);
#3494=ORIENTED_EDGE('',*,*,#2803,.F.);
#3495=ORIENTED_EDGE('',*,*,#2799,.F.);
#3496=ORIENTED_EDGE('',*,*,#2804,.F.);
#3497=ORIENTED_EDGE('',*,*,#2805,.T.);
#3498=ORIENTED_EDGE('',*,*,#2806,.F.);
#3499=ORIENTED_EDGE('',*,*,#2802,.F.);
#3500=ORIENTED_EDGE('',*,*,#2807,.F.);
#3501=ORIENTED_EDGE('',*,*,#2808,.F.);
#3502=ORIENTED_EDGE('',*,*,#2809,.F.);
#3503=ORIENTED_EDGE('',*,*,#2805,.F.);
#3504=ORIENTED_EDGE('',*,*,#2810,.F.);
#3505=ORIENTED_EDGE('',*,*,#2811,.T.);
#3506=ORIENTED_EDGE('',*,*,#2812,.F.);
#3507=ORIENTED_EDGE('',*,*,#2813,.F.);
#3508=ORIENTED_EDGE('',*,*,#2814,.F.);
#3509=ORIENTED_EDGE('',*,*,#2815,.T.);
#3510=ORIENTED_EDGE('',*,*,#2816,.F.);
#3511=ORIENTED_EDGE('',*,*,#2811,.F.);
#3512=ORIENTED_EDGE('',*,*,#2817,.F.);
#3513=ORIENTED_EDGE('',*,*,#2818,.T.);
#3514=ORIENTED_EDGE('',*,*,#2819,.F.);
#3515=ORIENTED_EDGE('',*,*,#2815,.F.);
#3516=ORIENTED_EDGE('',*,*,#2820,.F.);
#3517=ORIENTED_EDGE('',*,*,#2821,.T.);
#3518=ORIENTED_EDGE('',*,*,#2822,.F.);
#3519=ORIENTED_EDGE('',*,*,#2818,.F.);
#3520=ORIENTED_EDGE('',*,*,#2823,.F.);
#3521=ORIENTED_EDGE('',*,*,#2824,.T.);
#3522=ORIENTED_EDGE('',*,*,#2825,.F.);
#3523=ORIENTED_EDGE('',*,*,#2821,.F.);
#3524=ORIENTED_EDGE('',*,*,#2826,.F.);
#3525=ORIENTED_EDGE('',*,*,#2827,.T.);
#3526=ORIENTED_EDGE('',*,*,#2828,.F.);
#3527=ORIENTED_EDGE('',*,*,#2824,.F.);
#3528=ORIENTED_EDGE('',*,*,#2829,.F.);
#3529=ORIENTED_EDGE('',*,*,#2830,.T.);
#3530=ORIENTED_EDGE('',*,*,#2831,.F.);
#3531=ORIENTED_EDGE('',*,*,#2827,.F.);
#3532=ORIENTED_EDGE('',*,*,#2832,.F.);
#3533=ORIENTED_EDGE('',*,*,#2833,.T.);
#3534=ORIENTED_EDGE('',*,*,#2834,.F.);
#3535=ORIENTED_EDGE('',*,*,#2830,.F.);
#3536=ORIENTED_EDGE('',*,*,#2835,.F.);
#3537=ORIENTED_EDGE('',*,*,#2836,.F.);
#3538=ORIENTED_EDGE('',*,*,#2837,.F.);
#3539=ORIENTED_EDGE('',*,*,#2833,.F.);
#3540=ORIENTED_EDGE('',*,*,#2838,.F.);
#3541=ORIENTED_EDGE('',*,*,#2839,.T.);
#3542=ORIENTED_EDGE('',*,*,#2840,.F.);
#3543=ORIENTED_EDGE('',*,*,#2841,.F.);
#3544=ORIENTED_EDGE('',*,*,#2842,.F.);
#3545=ORIENTED_EDGE('',*,*,#2843,.T.);
#3546=ORIENTED_EDGE('',*,*,#2844,.F.);
#3547=ORIENTED_EDGE('',*,*,#2839,.F.);
#3548=ORIENTED_EDGE('',*,*,#2845,.F.);
#3549=ORIENTED_EDGE('',*,*,#2846,.T.);
#3550=ORIENTED_EDGE('',*,*,#2847,.F.);
#3551=ORIENTED_EDGE('',*,*,#2843,.F.);
#3552=ORIENTED_EDGE('',*,*,#2848,.F.);
#3553=ORIENTED_EDGE('',*,*,#2849,.T.);
#3554=ORIENTED_EDGE('',*,*,#2850,.F.);
#3555=ORIENTED_EDGE('',*,*,#2846,.F.);
#3556=ORIENTED_EDGE('',*,*,#2851,.F.);
#3557=ORIENTED_EDGE('',*,*,#2852,.T.);
#3558=ORIENTED_EDGE('',*,*,#2853,.F.);
#3559=ORIENTED_EDGE('',*,*,#2849,.F.);
#3560=ORIENTED_EDGE('',*,*,#2854,.F.);
#3561=ORIENTED_EDGE('',*,*,#2855,.T.);
#3562=ORIENTED_EDGE('',*,*,#2856,.F.);
#3563=ORIENTED_EDGE('',*,*,#2852,.F.);
#3564=ORIENTED_EDGE('',*,*,#2857,.F.);
#3565=ORIENTED_EDGE('',*,*,#2858,.T.);
#3566=ORIENTED_EDGE('',*,*,#2859,.F.);
#3567=ORIENTED_EDGE('',*,*,#2855,.F.);
#3568=ORIENTED_EDGE('',*,*,#2860,.F.);
#3569=ORIENTED_EDGE('',*,*,#2861,.T.);
#3570=ORIENTED_EDGE('',*,*,#2862,.F.);
#3571=ORIENTED_EDGE('',*,*,#2858,.F.);
#3572=ORIENTED_EDGE('',*,*,#2863,.F.);
#3573=ORIENTED_EDGE('',*,*,#2864,.F.);
#3574=ORIENTED_EDGE('',*,*,#2865,.F.);
#3575=ORIENTED_EDGE('',*,*,#2861,.F.);
#3576=ORIENTED_EDGE('',*,*,#2866,.F.);
#3577=ORIENTED_EDGE('',*,*,#2867,.T.);
#3578=ORIENTED_EDGE('',*,*,#2868,.F.);
#3579=ORIENTED_EDGE('',*,*,#2869,.F.);
#3580=ORIENTED_EDGE('',*,*,#2870,.F.);
#3581=ORIENTED_EDGE('',*,*,#2871,.T.);
#3582=ORIENTED_EDGE('',*,*,#2872,.F.);
#3583=ORIENTED_EDGE('',*,*,#2867,.F.);
#3584=ORIENTED_EDGE('',*,*,#2873,.F.);
#3585=ORIENTED_EDGE('',*,*,#2874,.T.);
#3586=ORIENTED_EDGE('',*,*,#2875,.F.);
#3587=ORIENTED_EDGE('',*,*,#2871,.F.);
#3588=ORIENTED_EDGE('',*,*,#2876,.F.);
#3589=ORIENTED_EDGE('',*,*,#2877,.T.);
#3590=ORIENTED_EDGE('',*,*,#2878,.F.);
#3591=ORIENTED_EDGE('',*,*,#2874,.F.);
#3592=ORIENTED_EDGE('',*,*,#2879,.F.);
#3593=ORIENTED_EDGE('',*,*,#2880,.T.);
#3594=ORIENTED_EDGE('',*,*,#2881,.F.);
#3595=ORIENTED_EDGE('',*,*,#2877,.F.);
#3596=ORIENTED_EDGE('',*,*,#2882,.F.);
#3597=ORIENTED_EDGE('',*,*,#2883,.T.);
#3598=ORIENTED_EDGE('',*,*,#2884,.F.);
#3599=ORIENTED_EDGE('',*,*,#2880,.F.);
#3600=ORIENTED_EDGE('',*,*,#2885,.F.);
#3601=ORIENTED_EDGE('',*,*,#2886,.T.);
#3602=ORIENTED_EDGE('',*,*,#2887,.F.);
#3603=ORIENTED_EDGE('',*,*,#2883,.F.);
#3604=ORIENTED_EDGE('',*,*,#2888,.F.);
#3605=ORIENTED_EDGE('',*,*,#2889,.T.);
#3606=ORIENTED_EDGE('',*,*,#2890,.F.);
#3607=ORIENTED_EDGE('',*,*,#2886,.F.);
#3608=ORIENTED_EDGE('',*,*,#2891,.F.);
#3609=ORIENTED_EDGE('',*,*,#2892,.F.);
#3610=ORIENTED_EDGE('',*,*,#2893,.F.);
#3611=ORIENTED_EDGE('',*,*,#2889,.F.);
#3612=ORIENTED_EDGE('',*,*,#2894,.F.);
#3613=ORIENTED_EDGE('',*,*,#2895,.T.);
#3614=ORIENTED_EDGE('',*,*,#2896,.F.);
#3615=ORIENTED_EDGE('',*,*,#2895,.F.);
#3616=ORIENTED_EDGE('',*,*,#2808,.T.);
#3617=ORIENTED_EDGE('',*,*,#2897,.T.);
#3618=ORIENTED_EDGE('',*,*,#2898,.T.);
#3619=ORIENTED_EDGE('',*,*,#2899,.F.);
#3620=ORIENTED_EDGE('',*,*,#2785,.T.);
#3621=ORIENTED_EDGE('',*,*,#2900,.F.);
#3622=ORIENTED_EDGE('',*,*,#2901,.F.);
#3623=ORIENTED_EDGE('',*,*,#2902,.T.);
#3624=ORIENTED_EDGE('',*,*,#2836,.T.);
#3625=ORIENTED_EDGE('',*,*,#2903,.T.);
#3626=ORIENTED_EDGE('',*,*,#2901,.T.);
#3627=ORIENTED_EDGE('',*,*,#2904,.F.);
#3628=ORIENTED_EDGE('',*,*,#2813,.T.);
#3629=ORIENTED_EDGE('',*,*,#2905,.F.);
#3630=ORIENTED_EDGE('',*,*,#2906,.F.);
#3631=ORIENTED_EDGE('',*,*,#2907,.T.);
#3632=ORIENTED_EDGE('',*,*,#2864,.T.);
#3633=ORIENTED_EDGE('',*,*,#2908,.T.);
#3634=ORIENTED_EDGE('',*,*,#2906,.T.);
#3635=ORIENTED_EDGE('',*,*,#2909,.F.);
#3636=ORIENTED_EDGE('',*,*,#2841,.T.);
#3637=ORIENTED_EDGE('',*,*,#2910,.F.);
#3638=ORIENTED_EDGE('',*,*,#2911,.F.);
#3639=ORIENTED_EDGE('',*,*,#2912,.T.);
#3640=ORIENTED_EDGE('',*,*,#2892,.T.);
#3641=ORIENTED_EDGE('',*,*,#2913,.T.);
#3642=ORIENTED_EDGE('',*,*,#2911,.T.);
#3643=ORIENTED_EDGE('',*,*,#2914,.F.);
#3644=ORIENTED_EDGE('',*,*,#2869,.T.);
#3645=ORIENTED_EDGE('',*,*,#2915,.F.);
#3646=ORIENTED_EDGE('',*,*,#2898,.F.);
#3647=ORIENTED_EDGE('',*,*,#2916,.T.);
#3648=ORIENTED_EDGE('',*,*,#2784,.T.);
#3649=ORIENTED_EDGE('',*,*,#2788,.T.);
#3650=ORIENTED_EDGE('',*,*,#2791,.T.);
#3651=ORIENTED_EDGE('',*,*,#2794,.T.);
#3652=ORIENTED_EDGE('',*,*,#2797,.T.);
#3653=ORIENTED_EDGE('',*,*,#2800,.T.);
#3654=ORIENTED_EDGE('',*,*,#2803,.T.);
#3655=ORIENTED_EDGE('',*,*,#2806,.T.);
#3656=ORIENTED_EDGE('',*,*,#2809,.T.);
#3657=ORIENTED_EDGE('',*,*,#2899,.T.);
#3658=ORIENTED_EDGE('',*,*,#2915,.T.);
#3659=ORIENTED_EDGE('',*,*,#2868,.T.);
#3660=ORIENTED_EDGE('',*,*,#2872,.T.);
#3661=ORIENTED_EDGE('',*,*,#2875,.T.);
#3662=ORIENTED_EDGE('',*,*,#2878,.T.);
#3663=ORIENTED_EDGE('',*,*,#2881,.T.);
#3664=ORIENTED_EDGE('',*,*,#2884,.T.);
#3665=ORIENTED_EDGE('',*,*,#2887,.T.);
#3666=ORIENTED_EDGE('',*,*,#2890,.T.);
#3667=ORIENTED_EDGE('',*,*,#2893,.T.);
#3668=ORIENTED_EDGE('',*,*,#2914,.T.);
#3669=ORIENTED_EDGE('',*,*,#2910,.T.);
#3670=ORIENTED_EDGE('',*,*,#2840,.T.);
#3671=ORIENTED_EDGE('',*,*,#2844,.T.);
#3672=ORIENTED_EDGE('',*,*,#2847,.T.);
#3673=ORIENTED_EDGE('',*,*,#2850,.T.);
#3674=ORIENTED_EDGE('',*,*,#2853,.T.);
#3675=ORIENTED_EDGE('',*,*,#2856,.T.);
#3676=ORIENTED_EDGE('',*,*,#2859,.T.);
#3677=ORIENTED_EDGE('',*,*,#2862,.T.);
#3678=ORIENTED_EDGE('',*,*,#2865,.T.);
#3679=ORIENTED_EDGE('',*,*,#2909,.T.);
#3680=ORIENTED_EDGE('',*,*,#2905,.T.);
#3681=ORIENTED_EDGE('',*,*,#2812,.T.);
#3682=ORIENTED_EDGE('',*,*,#2816,.T.);
#3683=ORIENTED_EDGE('',*,*,#2819,.T.);
#3684=ORIENTED_EDGE('',*,*,#2822,.T.);
#3685=ORIENTED_EDGE('',*,*,#2825,.T.);
#3686=ORIENTED_EDGE('',*,*,#2828,.T.);
#3687=ORIENTED_EDGE('',*,*,#2831,.T.);
#3688=ORIENTED_EDGE('',*,*,#2834,.T.);
#3689=ORIENTED_EDGE('',*,*,#2837,.T.);
#3690=ORIENTED_EDGE('',*,*,#2904,.T.);
#3691=ORIENTED_EDGE('',*,*,#2900,.T.);
#3692=ORIENTED_EDGE('',*,*,#2896,.T.);
#3693=ORIENTED_EDGE('',*,*,#2782,.T.);
#3694=ORIENTED_EDGE('',*,*,#2902,.F.);
#3695=ORIENTED_EDGE('',*,*,#2903,.F.);
#3696=ORIENTED_EDGE('',*,*,#2835,.T.);
#3697=ORIENTED_EDGE('',*,*,#2832,.T.);
#3698=ORIENTED_EDGE('',*,*,#2829,.T.);
#3699=ORIENTED_EDGE('',*,*,#2826,.T.);
#3700=ORIENTED_EDGE('',*,*,#2823,.T.);
#3701=ORIENTED_EDGE('',*,*,#2820,.T.);
#3702=ORIENTED_EDGE('',*,*,#2817,.T.);
#3703=ORIENTED_EDGE('',*,*,#2814,.T.);
#3704=ORIENTED_EDGE('',*,*,#2810,.T.);
#3705=ORIENTED_EDGE('',*,*,#2907,.F.);
#3706=ORIENTED_EDGE('',*,*,#2908,.F.);
#3707=ORIENTED_EDGE('',*,*,#2863,.T.);
#3708=ORIENTED_EDGE('',*,*,#2860,.T.);
#3709=ORIENTED_EDGE('',*,*,#2857,.T.);
#3710=ORIENTED_EDGE('',*,*,#2854,.T.);
#3711=ORIENTED_EDGE('',*,*,#2851,.T.);
#3712=ORIENTED_EDGE('',*,*,#2848,.T.);
#3713=ORIENTED_EDGE('',*,*,#2845,.T.);
#3714=ORIENTED_EDGE('',*,*,#2842,.T.);
#3715=ORIENTED_EDGE('',*,*,#2838,.T.);
#3716=ORIENTED_EDGE('',*,*,#2912,.F.);
#3717=ORIENTED_EDGE('',*,*,#2913,.F.);
#3718=ORIENTED_EDGE('',*,*,#2891,.T.);
#3719=ORIENTED_EDGE('',*,*,#2888,.T.);
#3720=ORIENTED_EDGE('',*,*,#2885,.T.);
#3721=ORIENTED_EDGE('',*,*,#2882,.T.);
#3722=ORIENTED_EDGE('',*,*,#2879,.T.);
#3723=ORIENTED_EDGE('',*,*,#2876,.T.);
#3724=ORIENTED_EDGE('',*,*,#2873,.T.);
#3725=ORIENTED_EDGE('',*,*,#2870,.T.);
#3726=ORIENTED_EDGE('',*,*,#2866,.T.);
#3727=ORIENTED_EDGE('',*,*,#2916,.F.);
#3728=ORIENTED_EDGE('',*,*,#2897,.F.);
#3729=ORIENTED_EDGE('',*,*,#2807,.T.);
#3730=ORIENTED_EDGE('',*,*,#2804,.T.);
#3731=ORIENTED_EDGE('',*,*,#2801,.T.);
#3732=ORIENTED_EDGE('',*,*,#2798,.T.);
#3733=ORIENTED_EDGE('',*,*,#2795,.T.);
#3734=ORIENTED_EDGE('',*,*,#2792,.T.);
#3735=ORIENTED_EDGE('',*,*,#2789,.T.);
#3736=ORIENTED_EDGE('',*,*,#2786,.T.);
#3737=ORIENTED_EDGE('',*,*,#2894,.T.);
#3738=ORIENTED_EDGE('',*,*,#2917,.F.);
#3739=ORIENTED_EDGE('',*,*,#2918,.F.);
#3740=ORIENTED_EDGE('',*,*,#2919,.F.);
#3741=ORIENTED_EDGE('',*,*,#2920,.F.);
#3742=ORIENTED_EDGE('',*,*,#2919,.T.);
#3743=ORIENTED_EDGE('',*,*,#2921,.T.);
#3744=ORIENTED_EDGE('',*,*,#2922,.F.);
#3745=ORIENTED_EDGE('',*,*,#2923,.F.);
#3746=ORIENTED_EDGE('',*,*,#2924,.T.);
#3747=ORIENTED_EDGE('',*,*,#2925,.T.);
#3748=ORIENTED_EDGE('',*,*,#2926,.T.);
#3749=ORIENTED_EDGE('',*,*,#2922,.T.);
#3750=ORIENTED_EDGE('',*,*,#2927,.T.);
#3751=ORIENTED_EDGE('',*,*,#2924,.F.);
#3752=ORIENTED_EDGE('',*,*,#2921,.F.);
#3753=ORIENTED_EDGE('',*,*,#2918,.T.);
#3754=ORIENTED_EDGE('',*,*,#2928,.F.);
#3755=ORIENTED_EDGE('',*,*,#2929,.F.);
#3756=ORIENTED_EDGE('',*,*,#2930,.T.);
#3757=ORIENTED_EDGE('',*,*,#2931,.F.);
#3758=ORIENTED_EDGE('',*,*,#2932,.T.);
#3759=ORIENTED_EDGE('',*,*,#2933,.T.);
#3760=ORIENTED_EDGE('',*,*,#2934,.T.);
#3761=ORIENTED_EDGE('',*,*,#2935,.T.);
#3762=ORIENTED_EDGE('',*,*,#2936,.T.);
#3763=ORIENTED_EDGE('',*,*,#2925,.F.);
#3764=ORIENTED_EDGE('',*,*,#2934,.F.);
#3765=ORIENTED_EDGE('',*,*,#2937,.F.);
#3766=ORIENTED_EDGE('',*,*,#2938,.F.);
#3767=ORIENTED_EDGE('',*,*,#2935,.F.);
#3768=ORIENTED_EDGE('',*,*,#2933,.F.);
#3769=ORIENTED_EDGE('',*,*,#2926,.F.);
#3770=ORIENTED_EDGE('',*,*,#2936,.F.);
#3771=ORIENTED_EDGE('',*,*,#2938,.T.);
#3772=ORIENTED_EDGE('',*,*,#2939,.F.);
#3773=ORIENTED_EDGE('',*,*,#2940,.F.);
#3774=ORIENTED_EDGE('',*,*,#2941,.T.);
#3775=ORIENTED_EDGE('',*,*,#2942,.F.);
#3776=ORIENTED_EDGE('',*,*,#2943,.T.);
#3777=ORIENTED_EDGE('',*,*,#2920,.T.);
#3778=ORIENTED_EDGE('',*,*,#2923,.T.);
#3779=ORIENTED_EDGE('',*,*,#2937,.T.);
#3780=ORIENTED_EDGE('',*,*,#2932,.F.);
#3781=ORIENTED_EDGE('',*,*,#2944,.F.);
#3782=ORIENTED_EDGE('',*,*,#2939,.T.);
#3783=ORIENTED_EDGE('',*,*,#2940,.T.);
#3784=ORIENTED_EDGE('',*,*,#2944,.T.);
#3785=ORIENTED_EDGE('',*,*,#2931,.T.);
#3786=ORIENTED_EDGE('',*,*,#2945,.T.);
#3787=ORIENTED_EDGE('',*,*,#2946,.T.);
#3788=ORIENTED_EDGE('',*,*,#2947,.T.);
#3789=ORIENTED_EDGE('',*,*,#2946,.F.);
#3790=ORIENTED_EDGE('',*,*,#2948,.F.);
#3791=ORIENTED_EDGE('',*,*,#2949,.T.);
#3792=ORIENTED_EDGE('',*,*,#2927,.F.);
#3793=ORIENTED_EDGE('',*,*,#2949,.F.);
#3794=ORIENTED_EDGE('',*,*,#2950,.F.);
#3795=ORIENTED_EDGE('',*,*,#2951,.F.);
#3796=ORIENTED_EDGE('',*,*,#2952,.F.);
#3797=ORIENTED_EDGE('',*,*,#2945,.F.);
#3798=ORIENTED_EDGE('',*,*,#2930,.F.);
#3799=ORIENTED_EDGE('',*,*,#2953,.F.);
#3800=ORIENTED_EDGE('',*,*,#2950,.T.);
#3801=ORIENTED_EDGE('',*,*,#2948,.T.);
#3802=ORIENTED_EDGE('',*,*,#2947,.F.);
#3803=ORIENTED_EDGE('',*,*,#2952,.T.);
#3804=ORIENTED_EDGE('',*,*,#2954,.F.);
#3805=ORIENTED_EDGE('',*,*,#2941,.F.);
#3806=ORIENTED_EDGE('',*,*,#2929,.T.);
#3807=ORIENTED_EDGE('',*,*,#2955,.T.);
#3808=ORIENTED_EDGE('',*,*,#2942,.T.);
#3809=ORIENTED_EDGE('',*,*,#2954,.T.);
#3810=ORIENTED_EDGE('',*,*,#2951,.T.);
#3811=ORIENTED_EDGE('',*,*,#2953,.T.);
#3812=ORIENTED_EDGE('',*,*,#2917,.T.);
#3813=ORIENTED_EDGE('',*,*,#2943,.F.);
#3814=ORIENTED_EDGE('',*,*,#2955,.F.);
#3815=ORIENTED_EDGE('',*,*,#2928,.T.);
#3816=ORIENTED_EDGE('',*,*,#2956,.T.);
#3817=ORIENTED_EDGE('',*,*,#2957,.T.);
#3818=ORIENTED_EDGE('',*,*,#2958,.T.);
#3819=ORIENTED_EDGE('',*,*,#2959,.F.);
#3820=ORIENTED_EDGE('',*,*,#2960,.T.);
#3821=ORIENTED_EDGE('',*,*,#2961,.T.);
#3822=ORIENTED_EDGE('',*,*,#2962,.T.);
#3823=ORIENTED_EDGE('',*,*,#2957,.F.);
#3824=ORIENTED_EDGE('',*,*,#2963,.T.);
#3825=ORIENTED_EDGE('',*,*,#2964,.T.);
#3826=ORIENTED_EDGE('',*,*,#2965,.T.);
#3827=ORIENTED_EDGE('',*,*,#2961,.F.);
#3828=ORIENTED_EDGE('',*,*,#2966,.T.);
#3829=ORIENTED_EDGE('',*,*,#2967,.T.);
#3830=ORIENTED_EDGE('',*,*,#2968,.T.);
#3831=ORIENTED_EDGE('',*,*,#2964,.F.);
#3832=ORIENTED_EDGE('',*,*,#2969,.T.);
#3833=ORIENTED_EDGE('',*,*,#2970,.T.);
#3834=ORIENTED_EDGE('',*,*,#2971,.T.);
#3835=ORIENTED_EDGE('',*,*,#2967,.F.);
#3836=ORIENTED_EDGE('',*,*,#2972,.T.);
#3837=ORIENTED_EDGE('',*,*,#2959,.T.);
#3838=ORIENTED_EDGE('',*,*,#2973,.T.);
#3839=ORIENTED_EDGE('',*,*,#2970,.F.);
#3840=ORIENTED_EDGE('',*,*,#2972,.F.);
#3841=ORIENTED_EDGE('',*,*,#2969,.F.);
#3842=ORIENTED_EDGE('',*,*,#2966,.F.);
#3843=ORIENTED_EDGE('',*,*,#2963,.F.);
#3844=ORIENTED_EDGE('',*,*,#2960,.F.);
#3845=ORIENTED_EDGE('',*,*,#2956,.F.);
#3846=ORIENTED_EDGE('',*,*,#2973,.F.);
#3847=ORIENTED_EDGE('',*,*,#2958,.F.);
#3848=ORIENTED_EDGE('',*,*,#2962,.F.);
#3849=ORIENTED_EDGE('',*,*,#2965,.F.);
#3850=ORIENTED_EDGE('',*,*,#2968,.F.);
#3851=ORIENTED_EDGE('',*,*,#2971,.F.);
#3852=ORIENTED_EDGE('',*,*,#2974,.F.);
#3853=ORIENTED_EDGE('',*,*,#2975,.F.);
#3854=ORIENTED_EDGE('',*,*,#2976,.F.);
#3855=ORIENTED_EDGE('',*,*,#2977,.T.);
#3856=ORIENTED_EDGE('',*,*,#2975,.T.);
#3857=ORIENTED_EDGE('',*,*,#2977,.F.);
#3858=ORIENTED_EDGE('',*,*,#2978,.F.);
#3859=ORIENTED_EDGE('',*,*,#2979,.T.);
#3860=ORIENTED_EDGE('',*,*,#2976,.T.);
#3861=ORIENTED_EDGE('',*,*,#2979,.F.);
#3862=ORIENTED_EDGE('',*,*,#2980,.F.);
#3863=ORIENTED_EDGE('',*,*,#2981,.T.);
#3864=ORIENTED_EDGE('',*,*,#2978,.T.);
#3865=ORIENTED_EDGE('',*,*,#2981,.F.);
#3866=ORIENTED_EDGE('',*,*,#2980,.T.);
#3867=ORIENTED_EDGE('',*,*,#2982,.F.);
#3868=ORIENTED_EDGE('',*,*,#2983,.F.);
#3869=ORIENTED_EDGE('',*,*,#2984,.T.);
#3870=ORIENTED_EDGE('',*,*,#2982,.T.);
#3871=ORIENTED_EDGE('',*,*,#2984,.F.);
#3872=ORIENTED_EDGE('',*,*,#2974,.T.);
#3873=ORIENTED_EDGE('',*,*,#2985,.T.);
#3874=ORIENTED_EDGE('',*,*,#2983,.T.);
#3875=ORIENTED_EDGE('',*,*,#2985,.F.);
#3876=ORIENTED_EDGE('',*,*,#2986,.F.);
#3877=ORIENTED_EDGE('',*,*,#2987,.T.);
#3878=ORIENTED_EDGE('',*,*,#2988,.F.);
#3879=ORIENTED_EDGE('',*,*,#2987,.F.);
#3880=ORIENTED_EDGE('',*,*,#2986,.T.);
#3881=ORIENTED_EDGE('',*,*,#2989,.F.);
#3882=ORIENTED_EDGE('',*,*,#2990,.F.);
#3883=ORIENTED_EDGE('',*,*,#2991,.T.);
#3884=ORIENTED_EDGE('',*,*,#2992,.F.);
#3885=ORIENTED_EDGE('',*,*,#2991,.F.);
#3886=ORIENTED_EDGE('',*,*,#2990,.T.);
#3887=ORIENTED_EDGE('',*,*,#2993,.F.);
#3888=ORIENTED_EDGE('',*,*,#2994,.F.);
#3889=ORIENTED_EDGE('',*,*,#2995,.T.);
#3890=ORIENTED_EDGE('',*,*,#2996,.F.);
#3891=ORIENTED_EDGE('',*,*,#2995,.F.);
#3892=ORIENTED_EDGE('',*,*,#2994,.T.);
#3893=ORIENTED_EDGE('',*,*,#2997,.F.);
#3894=ORIENTED_EDGE('',*,*,#2998,.F.);
#3895=ORIENTED_EDGE('',*,*,#2999,.T.);
#3896=ORIENTED_EDGE('',*,*,#3000,.F.);
#3897=ORIENTED_EDGE('',*,*,#2999,.F.);
#3898=ORIENTED_EDGE('',*,*,#2998,.T.);
#3899=ORIENTED_EDGE('',*,*,#3001,.F.);
#3900=ORIENTED_EDGE('',*,*,#3002,.F.);
#3901=ORIENTED_EDGE('',*,*,#3003,.T.);
#3902=ORIENTED_EDGE('',*,*,#2989,.T.);
#3903=ORIENTED_EDGE('',*,*,#3003,.F.);
#3904=ORIENTED_EDGE('',*,*,#3004,.F.);
#3905=ORIENTED_EDGE('',*,*,#3005,.T.);
#3906=ORIENTED_EDGE('',*,*,#2993,.T.);
#3907=ORIENTED_EDGE('',*,*,#3005,.F.);
#3908=ORIENTED_EDGE('',*,*,#3006,.F.);
#3909=ORIENTED_EDGE('',*,*,#3007,.T.);
#3910=ORIENTED_EDGE('',*,*,#2997,.T.);
#3911=ORIENTED_EDGE('',*,*,#3007,.F.);
#3912=ORIENTED_EDGE('',*,*,#3008,.F.);
#3913=ORIENTED_EDGE('',*,*,#3009,.T.);
#3914=ORIENTED_EDGE('',*,*,#3001,.T.);
#3915=ORIENTED_EDGE('',*,*,#3009,.F.);
#3916=ORIENTED_EDGE('',*,*,#3010,.T.);
#3917=ORIENTED_EDGE('',*,*,#3011,.T.);
#3918=ORIENTED_EDGE('',*,*,#3012,.F.);
#3919=ORIENTED_EDGE('',*,*,#3013,.F.);
#3920=ORIENTED_EDGE('',*,*,#3014,.T.);
#3921=ORIENTED_EDGE('',*,*,#3013,.T.);
#3922=ORIENTED_EDGE('',*,*,#3015,.F.);
#3923=ORIENTED_EDGE('',*,*,#3016,.F.);
#3924=ORIENTED_EDGE('',*,*,#3017,.T.);
#3925=ORIENTED_EDGE('',*,*,#3016,.T.);
#3926=ORIENTED_EDGE('',*,*,#3018,.F.);
#3927=ORIENTED_EDGE('',*,*,#3019,.F.);
#3928=ORIENTED_EDGE('',*,*,#3020,.T.);
#3929=ORIENTED_EDGE('',*,*,#3019,.T.);
#3930=ORIENTED_EDGE('',*,*,#3021,.F.);
#3931=ORIENTED_EDGE('',*,*,#3022,.F.);
#3932=ORIENTED_EDGE('',*,*,#3023,.T.);
#3933=ORIENTED_EDGE('',*,*,#3022,.T.);
#3934=ORIENTED_EDGE('',*,*,#3024,.F.);
#3935=ORIENTED_EDGE('',*,*,#3025,.F.);
#3936=ORIENTED_EDGE('',*,*,#3000,.T.);
#3937=ORIENTED_EDGE('',*,*,#2996,.T.);
#3938=ORIENTED_EDGE('',*,*,#2992,.T.);
#3939=ORIENTED_EDGE('',*,*,#2988,.T.);
#3940=ORIENTED_EDGE('',*,*,#3026,.T.);
#3941=ORIENTED_EDGE('',*,*,#3025,.T.);
#3942=ORIENTED_EDGE('',*,*,#3027,.F.);
#3943=ORIENTED_EDGE('',*,*,#3028,.F.);
#3944=ORIENTED_EDGE('',*,*,#3029,.T.);
#3945=ORIENTED_EDGE('',*,*,#3028,.T.);
#3946=ORIENTED_EDGE('',*,*,#3030,.F.);
#3947=ORIENTED_EDGE('',*,*,#3031,.F.);
#3948=ORIENTED_EDGE('',*,*,#3032,.T.);
#3949=ORIENTED_EDGE('',*,*,#3031,.T.);
#3950=ORIENTED_EDGE('',*,*,#3033,.F.);
#3951=ORIENTED_EDGE('',*,*,#3034,.F.);
#3952=ORIENTED_EDGE('',*,*,#3035,.T.);
#3953=ORIENTED_EDGE('',*,*,#3034,.T.);
#3954=ORIENTED_EDGE('',*,*,#3036,.F.);
#3955=ORIENTED_EDGE('',*,*,#3037,.F.);
#3956=ORIENTED_EDGE('',*,*,#3038,.T.);
#3957=ORIENTED_EDGE('',*,*,#3037,.T.);
#3958=ORIENTED_EDGE('',*,*,#3039,.F.);
#3959=ORIENTED_EDGE('',*,*,#3040,.F.);
#3960=ORIENTED_EDGE('',*,*,#3041,.T.);
#3961=ORIENTED_EDGE('',*,*,#3040,.T.);
#3962=ORIENTED_EDGE('',*,*,#3042,.F.);
#3963=ORIENTED_EDGE('',*,*,#3043,.F.);
#3964=ORIENTED_EDGE('',*,*,#3002,.T.);
#3965=ORIENTED_EDGE('',*,*,#3004,.T.);
#3966=ORIENTED_EDGE('',*,*,#3006,.T.);
#3967=ORIENTED_EDGE('',*,*,#3008,.T.);
#3968=ORIENTED_EDGE('',*,*,#3044,.T.);
#3969=ORIENTED_EDGE('',*,*,#3043,.T.);
#3970=ORIENTED_EDGE('',*,*,#3045,.F.);
#3971=ORIENTED_EDGE('',*,*,#3011,.F.);
#3972=ORIENTED_EDGE('',*,*,#3045,.T.);
#3973=ORIENTED_EDGE('',*,*,#3042,.T.);
#3974=ORIENTED_EDGE('',*,*,#3039,.T.);
#3975=ORIENTED_EDGE('',*,*,#3036,.T.);
#3976=ORIENTED_EDGE('',*,*,#3033,.T.);
#3977=ORIENTED_EDGE('',*,*,#3030,.T.);
#3978=ORIENTED_EDGE('',*,*,#3027,.T.);
#3979=ORIENTED_EDGE('',*,*,#3024,.T.);
#3980=ORIENTED_EDGE('',*,*,#3021,.T.);
#3981=ORIENTED_EDGE('',*,*,#3018,.T.);
#3982=ORIENTED_EDGE('',*,*,#3015,.T.);
#3983=ORIENTED_EDGE('',*,*,#3012,.T.);
#3984=ORIENTED_EDGE('',*,*,#3044,.F.);
#3985=ORIENTED_EDGE('',*,*,#3010,.F.);
#3986=ORIENTED_EDGE('',*,*,#3014,.F.);
#3987=ORIENTED_EDGE('',*,*,#3017,.F.);
#3988=ORIENTED_EDGE('',*,*,#3020,.F.);
#3989=ORIENTED_EDGE('',*,*,#3023,.F.);
#3990=ORIENTED_EDGE('',*,*,#3026,.F.);
#3991=ORIENTED_EDGE('',*,*,#3029,.F.);
#3992=ORIENTED_EDGE('',*,*,#3032,.F.);
#3993=ORIENTED_EDGE('',*,*,#3035,.F.);
#3994=ORIENTED_EDGE('',*,*,#3038,.F.);
#3995=ORIENTED_EDGE('',*,*,#3041,.F.);
#3996=ORIENTED_EDGE('',*,*,#3046,.F.);
#3997=ORIENTED_EDGE('',*,*,#3047,.F.);
#3998=ORIENTED_EDGE('',*,*,#3048,.T.);
#3999=ORIENTED_EDGE('',*,*,#3046,.T.);
#4000=ORIENTED_EDGE('',*,*,#3048,.F.);
#4001=ORIENTED_EDGE('',*,*,#3049,.F.);
#4002=ORIENTED_EDGE('',*,*,#3050,.T.);
#4003=ORIENTED_EDGE('',*,*,#3047,.T.);
#4004=ORIENTED_EDGE('',*,*,#3050,.F.);
#4005=ORIENTED_EDGE('',*,*,#3051,.F.);
#4006=ORIENTED_EDGE('',*,*,#3052,.T.);
#4007=ORIENTED_EDGE('',*,*,#3049,.T.);
#4008=ORIENTED_EDGE('',*,*,#3052,.F.);
#4009=ORIENTED_EDGE('',*,*,#3051,.T.);
#4010=ORIENTED_EDGE('',*,*,#3053,.F.);
#4011=ORIENTED_EDGE('',*,*,#3054,.F.);
#4012=ORIENTED_EDGE('',*,*,#3055,.T.);
#4013=ORIENTED_EDGE('',*,*,#3053,.T.);
#4014=ORIENTED_EDGE('',*,*,#3055,.F.);
#4015=ORIENTED_EDGE('',*,*,#3056,.F.);
#4016=ORIENTED_EDGE('',*,*,#3057,.T.);
#4017=ORIENTED_EDGE('',*,*,#3054,.T.);
#4018=ORIENTED_EDGE('',*,*,#3057,.F.);
#4019=ORIENTED_EDGE('',*,*,#3058,.F.);
#4020=ORIENTED_EDGE('',*,*,#3059,.T.);
#4021=ORIENTED_EDGE('',*,*,#3056,.T.);
#4022=ORIENTED_EDGE('',*,*,#3059,.F.);
#4023=ORIENTED_EDGE('',*,*,#3058,.T.);
#4024=ORIENTED_EDGE('',*,*,#3060,.T.);
#4025=ORIENTED_EDGE('',*,*,#3061,.T.);
#4026=ORIENTED_EDGE('',*,*,#3062,.T.);
#4027=ORIENTED_EDGE('',*,*,#3063,.F.);
#4028=ORIENTED_EDGE('',*,*,#3064,.T.);
#4029=ORIENTED_EDGE('',*,*,#3065,.T.);
#4030=ORIENTED_EDGE('',*,*,#3066,.T.);
#4031=ORIENTED_EDGE('',*,*,#3061,.F.);
#4032=ORIENTED_EDGE('',*,*,#3067,.T.);
#4033=ORIENTED_EDGE('',*,*,#3068,.T.);
#4034=ORIENTED_EDGE('',*,*,#3069,.T.);
#4035=ORIENTED_EDGE('',*,*,#3065,.F.);
#4036=ORIENTED_EDGE('',*,*,#3070,.T.);
#4037=ORIENTED_EDGE('',*,*,#3071,.T.);
#4038=ORIENTED_EDGE('',*,*,#3072,.T.);
#4039=ORIENTED_EDGE('',*,*,#3068,.F.);
#4040=ORIENTED_EDGE('',*,*,#3073,.T.);
#4041=ORIENTED_EDGE('',*,*,#3074,.T.);
#4042=ORIENTED_EDGE('',*,*,#3075,.T.);
#4043=ORIENTED_EDGE('',*,*,#3071,.F.);
#4044=ORIENTED_EDGE('',*,*,#3076,.T.);
#4045=ORIENTED_EDGE('',*,*,#3063,.T.);
#4046=ORIENTED_EDGE('',*,*,#3077,.T.);
#4047=ORIENTED_EDGE('',*,*,#3074,.F.);
#4048=ORIENTED_EDGE('',*,*,#3076,.F.);
#4049=ORIENTED_EDGE('',*,*,#3073,.F.);
#4050=ORIENTED_EDGE('',*,*,#3070,.F.);
#4051=ORIENTED_EDGE('',*,*,#3067,.F.);
#4052=ORIENTED_EDGE('',*,*,#3064,.F.);
#4053=ORIENTED_EDGE('',*,*,#3060,.F.);
#4054=ORIENTED_EDGE('',*,*,#3077,.F.);
#4055=ORIENTED_EDGE('',*,*,#3062,.F.);
#4056=ORIENTED_EDGE('',*,*,#3066,.F.);
#4057=ORIENTED_EDGE('',*,*,#3069,.F.);
#4058=ORIENTED_EDGE('',*,*,#3072,.F.);
#4059=ORIENTED_EDGE('',*,*,#3075,.F.);
#4060=ORIENTED_EDGE('',*,*,#3078,.F.);
#4061=ORIENTED_EDGE('',*,*,#3079,.T.);
#4062=ORIENTED_EDGE('',*,*,#3080,.F.);
#4063=ORIENTED_EDGE('',*,*,#3079,.F.);
#4064=ORIENTED_EDGE('',*,*,#3078,.T.);
#4065=ORIENTED_EDGE('',*,*,#3081,.F.);
#4066=ORIENTED_EDGE('',*,*,#3082,.F.);
#4067=ORIENTED_EDGE('',*,*,#3083,.T.);
#4068=ORIENTED_EDGE('',*,*,#3084,.F.);
#4069=ORIENTED_EDGE('',*,*,#3083,.F.);
#4070=ORIENTED_EDGE('',*,*,#3082,.T.);
#4071=ORIENTED_EDGE('',*,*,#3085,.F.);
#4072=ORIENTED_EDGE('',*,*,#3086,.F.);
#4073=ORIENTED_EDGE('',*,*,#3087,.T.);
#4074=ORIENTED_EDGE('',*,*,#3081,.T.);
#4075=ORIENTED_EDGE('',*,*,#3087,.F.);
#4076=ORIENTED_EDGE('',*,*,#3088,.F.);
#4077=ORIENTED_EDGE('',*,*,#3089,.T.);
#4078=ORIENTED_EDGE('',*,*,#3085,.T.);
#4079=ORIENTED_EDGE('',*,*,#3089,.F.);
#4080=ORIENTED_EDGE('',*,*,#3090,.T.);
#4081=ORIENTED_EDGE('',*,*,#3091,.T.);
#4082=ORIENTED_EDGE('',*,*,#3092,.F.);
#4083=ORIENTED_EDGE('',*,*,#3093,.F.);
#4084=ORIENTED_EDGE('',*,*,#3094,.T.);
#4085=ORIENTED_EDGE('',*,*,#3093,.T.);
#4086=ORIENTED_EDGE('',*,*,#3095,.F.);
#4087=ORIENTED_EDGE('',*,*,#3096,.F.);
#4088=ORIENTED_EDGE('',*,*,#3097,.T.);
#4089=ORIENTED_EDGE('',*,*,#3096,.T.);
#4090=ORIENTED_EDGE('',*,*,#3098,.F.);
#4091=ORIENTED_EDGE('',*,*,#3099,.F.);
#4092=ORIENTED_EDGE('',*,*,#3100,.T.);
#4093=ORIENTED_EDGE('',*,*,#3099,.T.);
#4094=ORIENTED_EDGE('',*,*,#3101,.F.);
#4095=ORIENTED_EDGE('',*,*,#3091,.F.);
#4096=ORIENTED_EDGE('',*,*,#3101,.T.);
#4097=ORIENTED_EDGE('',*,*,#3098,.T.);
#4098=ORIENTED_EDGE('',*,*,#3095,.T.);
#4099=ORIENTED_EDGE('',*,*,#3092,.T.);
#4100=ORIENTED_EDGE('',*,*,#3080,.T.);
#4101=ORIENTED_EDGE('',*,*,#3084,.T.);
#4102=ORIENTED_EDGE('',*,*,#3100,.F.);
#4103=ORIENTED_EDGE('',*,*,#3090,.F.);
#4104=ORIENTED_EDGE('',*,*,#3094,.F.);
#4105=ORIENTED_EDGE('',*,*,#3097,.F.);
#4106=ORIENTED_EDGE('',*,*,#3086,.T.);
#4107=ORIENTED_EDGE('',*,*,#3088,.T.);
#4108=ORIENTED_EDGE('',*,*,#3102,.T.);
#4109=ORIENTED_EDGE('',*,*,#3103,.T.);
#4110=ORIENTED_EDGE('',*,*,#3104,.F.);
#4111=ORIENTED_EDGE('',*,*,#3105,.F.);
#4112=ORIENTED_EDGE('',*,*,#3106,.T.);
#4113=ORIENTED_EDGE('',*,*,#3105,.T.);
#4114=ORIENTED_EDGE('',*,*,#3107,.F.);
#4115=ORIENTED_EDGE('',*,*,#3108,.F.);
#4116=ORIENTED_EDGE('',*,*,#3109,.T.);
#4117=ORIENTED_EDGE('',*,*,#3108,.T.);
#4118=ORIENTED_EDGE('',*,*,#3110,.F.);
#4119=ORIENTED_EDGE('',*,*,#3111,.F.);
#4120=ORIENTED_EDGE('',*,*,#3112,.T.);
#4121=ORIENTED_EDGE('',*,*,#3111,.T.);
#4122=ORIENTED_EDGE('',*,*,#3113,.F.);
#4123=ORIENTED_EDGE('',*,*,#3103,.F.);
#4124=ORIENTED_EDGE('',*,*,#3113,.T.);
#4125=ORIENTED_EDGE('',*,*,#3110,.T.);
#4126=ORIENTED_EDGE('',*,*,#3107,.T.);
#4127=ORIENTED_EDGE('',*,*,#3104,.T.);
#4128=ORIENTED_EDGE('',*,*,#3112,.F.);
#4129=ORIENTED_EDGE('',*,*,#3102,.F.);
#4130=ORIENTED_EDGE('',*,*,#3106,.F.);
#4131=ORIENTED_EDGE('',*,*,#3109,.F.);
#4132=ORIENTED_EDGE('',*,*,#3114,.T.);
#4133=ORIENTED_EDGE('',*,*,#3115,.T.);
#4134=ORIENTED_EDGE('',*,*,#3116,.F.);
#4135=ORIENTED_EDGE('',*,*,#3117,.F.);
#4136=ORIENTED_EDGE('',*,*,#3118,.T.);
#4137=ORIENTED_EDGE('',*,*,#3117,.T.);
#4138=ORIENTED_EDGE('',*,*,#3119,.F.);
#4139=ORIENTED_EDGE('',*,*,#3120,.F.);
#4140=ORIENTED_EDGE('',*,*,#3121,.T.);
#4141=ORIENTED_EDGE('',*,*,#3120,.T.);
#4142=ORIENTED_EDGE('',*,*,#3122,.F.);
#4143=ORIENTED_EDGE('',*,*,#3123,.F.);
#4144=ORIENTED_EDGE('',*,*,#3124,.T.);
#4145=ORIENTED_EDGE('',*,*,#3123,.T.);
#4146=ORIENTED_EDGE('',*,*,#3125,.F.);
#4147=ORIENTED_EDGE('',*,*,#3115,.F.);
#4148=ORIENTED_EDGE('',*,*,#3125,.T.);
#4149=ORIENTED_EDGE('',*,*,#3122,.T.);
#4150=ORIENTED_EDGE('',*,*,#3119,.T.);
#4151=ORIENTED_EDGE('',*,*,#3116,.T.);
#4152=ORIENTED_EDGE('',*,*,#3124,.F.);
#4153=ORIENTED_EDGE('',*,*,#3114,.F.);
#4154=ORIENTED_EDGE('',*,*,#3118,.F.);
#4155=ORIENTED_EDGE('',*,*,#3121,.F.);
#4156=ORIENTED_EDGE('',*,*,#3126,.F.);
#4157=ORIENTED_EDGE('',*,*,#3127,.T.);
#4158=ORIENTED_EDGE('',*,*,#3128,.F.);
#4159=ORIENTED_EDGE('',*,*,#3129,.F.);
#4160=ORIENTED_EDGE('',*,*,#3130,.T.);
#4161=ORIENTED_EDGE('',*,*,#3131,.F.);
#4162=ORIENTED_EDGE('',*,*,#3130,.F.);
#4163=ORIENTED_EDGE('',*,*,#3132,.F.);
#4164=ORIENTED_EDGE('',*,*,#3133,.F.);
#4165=ORIENTED_EDGE('',*,*,#3127,.F.);
#4166=ORIENTED_EDGE('',*,*,#3134,.F.);
#4167=ORIENTED_EDGE('',*,*,#3135,.T.);
#4168=ORIENTED_EDGE('',*,*,#3136,.F.);
#4169=ORIENTED_EDGE('',*,*,#3137,.F.);
#4170=ORIENTED_EDGE('',*,*,#3138,.T.);
#4171=ORIENTED_EDGE('',*,*,#3139,.F.);
#4172=ORIENTED_EDGE('',*,*,#3138,.F.);
#4173=ORIENTED_EDGE('',*,*,#3140,.F.);
#4174=ORIENTED_EDGE('',*,*,#3141,.F.);
#4175=ORIENTED_EDGE('',*,*,#3135,.F.);
#4176=ORIENTED_EDGE('',*,*,#3142,.F.);
#4177=ORIENTED_EDGE('',*,*,#3143,.T.);
#4178=ORIENTED_EDGE('',*,*,#3144,.F.);
#4179=ORIENTED_EDGE('',*,*,#3145,.F.);
#4180=ORIENTED_EDGE('',*,*,#3146,.T.);
#4181=ORIENTED_EDGE('',*,*,#3147,.F.);
#4182=ORIENTED_EDGE('',*,*,#3146,.F.);
#4183=ORIENTED_EDGE('',*,*,#3148,.F.);
#4184=ORIENTED_EDGE('',*,*,#3149,.F.);
#4185=ORIENTED_EDGE('',*,*,#3143,.F.);
#4186=ORIENTED_EDGE('',*,*,#3150,.F.);
#4187=ORIENTED_EDGE('',*,*,#3151,.T.);
#4188=ORIENTED_EDGE('',*,*,#3152,.F.);
#4189=ORIENTED_EDGE('',*,*,#3153,.F.);
#4190=ORIENTED_EDGE('',*,*,#3154,.T.);
#4191=ORIENTED_EDGE('',*,*,#3155,.F.);
#4192=ORIENTED_EDGE('',*,*,#3154,.F.);
#4193=ORIENTED_EDGE('',*,*,#3156,.F.);
#4194=ORIENTED_EDGE('',*,*,#3157,.F.);
#4195=ORIENTED_EDGE('',*,*,#3151,.F.);
#4196=ORIENTED_EDGE('',*,*,#3128,.T.);
#4197=ORIENTED_EDGE('',*,*,#3126,.T.);
#4198=ORIENTED_EDGE('',*,*,#3133,.T.);
#4199=ORIENTED_EDGE('',*,*,#3158,.T.);
#4200=ORIENTED_EDGE('',*,*,#3144,.T.);
#4201=ORIENTED_EDGE('',*,*,#3142,.T.);
#4202=ORIENTED_EDGE('',*,*,#3149,.T.);
#4203=ORIENTED_EDGE('',*,*,#3159,.T.);
#4204=ORIENTED_EDGE('',*,*,#3160,.F.);
#4205=ORIENTED_EDGE('',*,*,#3161,.T.);
#4206=ORIENTED_EDGE('',*,*,#3162,.F.);
#4207=ORIENTED_EDGE('',*,*,#3163,.T.);
#4208=ORIENTED_EDGE('',*,*,#3136,.T.);
#4209=ORIENTED_EDGE('',*,*,#3134,.T.);
#4210=ORIENTED_EDGE('',*,*,#3141,.T.);
#4211=ORIENTED_EDGE('',*,*,#3164,.T.);
#4212=ORIENTED_EDGE('',*,*,#3152,.T.);
#4213=ORIENTED_EDGE('',*,*,#3150,.T.);
#4214=ORIENTED_EDGE('',*,*,#3157,.T.);
#4215=ORIENTED_EDGE('',*,*,#3165,.T.);
#4216=ORIENTED_EDGE('',*,*,#3166,.F.);
#4217=ORIENTED_EDGE('',*,*,#3167,.F.);
#4218=ORIENTED_EDGE('',*,*,#3168,.F.);
#4219=ORIENTED_EDGE('',*,*,#3169,.T.);
#4220=ORIENTED_EDGE('',*,*,#3160,.T.);
#4221=ORIENTED_EDGE('',*,*,#3170,.T.);
#4222=ORIENTED_EDGE('',*,*,#3171,.T.);
#4223=ORIENTED_EDGE('',*,*,#3172,.T.);
#4224=ORIENTED_EDGE('',*,*,#3173,.T.);
#4225=ORIENTED_EDGE('',*,*,#3174,.T.);
#4226=ORIENTED_EDGE('',*,*,#3168,.T.);
#4227=ORIENTED_EDGE('',*,*,#3175,.T.);
#4228=ORIENTED_EDGE('',*,*,#3176,.T.);
#4229=ORIENTED_EDGE('',*,*,#3177,.T.);
#4230=ORIENTED_EDGE('',*,*,#3178,.T.);
#4231=ORIENTED_EDGE('',*,*,#3179,.T.);
#4232=ORIENTED_EDGE('',*,*,#3132,.T.);
#4233=ORIENTED_EDGE('',*,*,#3129,.T.);
#4234=ORIENTED_EDGE('',*,*,#3163,.F.);
#4235=ORIENTED_EDGE('',*,*,#3180,.F.);
#4236=ORIENTED_EDGE('',*,*,#3181,.F.);
#4237=ORIENTED_EDGE('',*,*,#3170,.F.);
#4238=ORIENTED_EDGE('',*,*,#3159,.F.);
#4239=ORIENTED_EDGE('',*,*,#3148,.T.);
#4240=ORIENTED_EDGE('',*,*,#3145,.T.);
#4241=ORIENTED_EDGE('',*,*,#3158,.F.);
#4242=ORIENTED_EDGE('',*,*,#3181,.T.);
#4243=ORIENTED_EDGE('',*,*,#3182,.F.);
#4244=ORIENTED_EDGE('',*,*,#3183,.F.);
#4245=ORIENTED_EDGE('',*,*,#3171,.F.);
#4246=ORIENTED_EDGE('',*,*,#3183,.T.);
#4247=ORIENTED_EDGE('',*,*,#3184,.F.);
#4248=ORIENTED_EDGE('',*,*,#3185,.F.);
#4249=ORIENTED_EDGE('',*,*,#3172,.F.);
#4250=ORIENTED_EDGE('',*,*,#3131,.T.);
#4251=ORIENTED_EDGE('',*,*,#3139,.T.);
#4252=ORIENTED_EDGE('',*,*,#3147,.T.);
#4253=ORIENTED_EDGE('',*,*,#3155,.T.);
#4254=ORIENTED_EDGE('',*,*,#3185,.T.);
#4255=ORIENTED_EDGE('',*,*,#3186,.F.);
#4256=ORIENTED_EDGE('',*,*,#3187,.F.);
#4257=ORIENTED_EDGE('',*,*,#3173,.F.);
#4258=ORIENTED_EDGE('',*,*,#3140,.T.);
#4259=ORIENTED_EDGE('',*,*,#3137,.T.);
#4260=ORIENTED_EDGE('',*,*,#3169,.F.);
#4261=ORIENTED_EDGE('',*,*,#3174,.F.);
#4262=ORIENTED_EDGE('',*,*,#3187,.T.);
#4263=ORIENTED_EDGE('',*,*,#3188,.F.);
#4264=ORIENTED_EDGE('',*,*,#3165,.F.);
#4265=ORIENTED_EDGE('',*,*,#3156,.T.);
#4266=ORIENTED_EDGE('',*,*,#3153,.T.);
#4267=ORIENTED_EDGE('',*,*,#3164,.F.);
#4268=ORIENTED_EDGE('',*,*,#3167,.T.);
#4269=ORIENTED_EDGE('',*,*,#3189,.F.);
#4270=ORIENTED_EDGE('',*,*,#3190,.F.);
#4271=ORIENTED_EDGE('',*,*,#3175,.F.);
#4272=ORIENTED_EDGE('',*,*,#3190,.T.);
#4273=ORIENTED_EDGE('',*,*,#3191,.F.);
#4274=ORIENTED_EDGE('',*,*,#3192,.F.);
#4275=ORIENTED_EDGE('',*,*,#3176,.F.);
#4276=ORIENTED_EDGE('',*,*,#3192,.T.);
#4277=ORIENTED_EDGE('',*,*,#3193,.F.);
#4278=ORIENTED_EDGE('',*,*,#3194,.F.);
#4279=ORIENTED_EDGE('',*,*,#3177,.F.);
#4280=ORIENTED_EDGE('',*,*,#3194,.T.);
#4281=ORIENTED_EDGE('',*,*,#3195,.F.);
#4282=ORIENTED_EDGE('',*,*,#3196,.F.);
#4283=ORIENTED_EDGE('',*,*,#3178,.F.);
#4284=ORIENTED_EDGE('',*,*,#3196,.T.);
#4285=ORIENTED_EDGE('',*,*,#3197,.F.);
#4286=ORIENTED_EDGE('',*,*,#3161,.F.);
#4287=ORIENTED_EDGE('',*,*,#3179,.F.);
#4288=ORIENTED_EDGE('',*,*,#3162,.T.);
#4289=ORIENTED_EDGE('',*,*,#3197,.T.);
#4290=ORIENTED_EDGE('',*,*,#3195,.T.);
#4291=ORIENTED_EDGE('',*,*,#3193,.T.);
#4292=ORIENTED_EDGE('',*,*,#3191,.T.);
#4293=ORIENTED_EDGE('',*,*,#3189,.T.);
#4294=ORIENTED_EDGE('',*,*,#3166,.T.);
#4295=ORIENTED_EDGE('',*,*,#3188,.T.);
#4296=ORIENTED_EDGE('',*,*,#3186,.T.);
#4297=ORIENTED_EDGE('',*,*,#3184,.T.);
#4298=ORIENTED_EDGE('',*,*,#3182,.T.);
#4299=ORIENTED_EDGE('',*,*,#3180,.T.);
#4300=ORIENTED_EDGE('',*,*,#3198,.T.);
#4301=ORIENTED_EDGE('',*,*,#3199,.T.);
#4302=ORIENTED_EDGE('',*,*,#3200,.F.);
#4303=ORIENTED_EDGE('',*,*,#3201,.F.);
#4304=ORIENTED_EDGE('',*,*,#3202,.T.);
#4305=ORIENTED_EDGE('',*,*,#3201,.T.);
#4306=ORIENTED_EDGE('',*,*,#3203,.F.);
#4307=ORIENTED_EDGE('',*,*,#3204,.F.);
#4308=ORIENTED_EDGE('',*,*,#3205,.T.);
#4309=ORIENTED_EDGE('',*,*,#3204,.T.);
#4310=ORIENTED_EDGE('',*,*,#3206,.F.);
#4311=ORIENTED_EDGE('',*,*,#3207,.F.);
#4312=ORIENTED_EDGE('',*,*,#3208,.T.);
#4313=ORIENTED_EDGE('',*,*,#3207,.T.);
#4314=ORIENTED_EDGE('',*,*,#3209,.F.);
#4315=ORIENTED_EDGE('',*,*,#3210,.F.);
#4316=ORIENTED_EDGE('',*,*,#3211,.T.);
#4317=ORIENTED_EDGE('',*,*,#3210,.T.);
#4318=ORIENTED_EDGE('',*,*,#3212,.F.);
#4319=ORIENTED_EDGE('',*,*,#3213,.F.);
#4320=ORIENTED_EDGE('',*,*,#3214,.T.);
#4321=ORIENTED_EDGE('',*,*,#3213,.T.);
#4322=ORIENTED_EDGE('',*,*,#3215,.F.);
#4323=ORIENTED_EDGE('',*,*,#3216,.F.);
#4324=ORIENTED_EDGE('',*,*,#3217,.T.);
#4325=ORIENTED_EDGE('',*,*,#3216,.T.);
#4326=ORIENTED_EDGE('',*,*,#3218,.F.);
#4327=ORIENTED_EDGE('',*,*,#3219,.F.);
#4328=ORIENTED_EDGE('',*,*,#3220,.T.);
#4329=ORIENTED_EDGE('',*,*,#3219,.T.);
#4330=ORIENTED_EDGE('',*,*,#3221,.F.);
#4331=ORIENTED_EDGE('',*,*,#3199,.F.);
#4332=ORIENTED_EDGE('',*,*,#3221,.T.);
#4333=ORIENTED_EDGE('',*,*,#3218,.T.);
#4334=ORIENTED_EDGE('',*,*,#3215,.T.);
#4335=ORIENTED_EDGE('',*,*,#3212,.T.);
#4336=ORIENTED_EDGE('',*,*,#3209,.T.);
#4337=ORIENTED_EDGE('',*,*,#3206,.T.);
#4338=ORIENTED_EDGE('',*,*,#3203,.T.);
#4339=ORIENTED_EDGE('',*,*,#3200,.T.);
#4340=ORIENTED_EDGE('',*,*,#3220,.F.);
#4341=ORIENTED_EDGE('',*,*,#3198,.F.);
#4342=ORIENTED_EDGE('',*,*,#3202,.F.);
#4343=ORIENTED_EDGE('',*,*,#3205,.F.);
#4344=ORIENTED_EDGE('',*,*,#3208,.F.);
#4345=ORIENTED_EDGE('',*,*,#3211,.F.);
#4346=ORIENTED_EDGE('',*,*,#3214,.F.);
#4347=ORIENTED_EDGE('',*,*,#3217,.F.);
#4348=ORIENTED_EDGE('',*,*,#3222,.F.);
#4349=ORIENTED_EDGE('',*,*,#3223,.T.);
#4350=ORIENTED_EDGE('',*,*,#3224,.F.);
#4351=ORIENTED_EDGE('',*,*,#3225,.F.);
#4352=ORIENTED_EDGE('',*,*,#3226,.F.);
#4353=ORIENTED_EDGE('',*,*,#3225,.T.);
#4354=ORIENTED_EDGE('',*,*,#3227,.F.);
#4355=ORIENTED_EDGE('',*,*,#3228,.F.);
#4356=ORIENTED_EDGE('',*,*,#3229,.F.);
#4357=ORIENTED_EDGE('',*,*,#3228,.T.);
#4358=ORIENTED_EDGE('',*,*,#3230,.F.);
#4359=ORIENTED_EDGE('',*,*,#3231,.F.);
#4360=ORIENTED_EDGE('',*,*,#3232,.F.);
#4361=ORIENTED_EDGE('',*,*,#3231,.T.);
#4362=ORIENTED_EDGE('',*,*,#3233,.F.);
#4363=ORIENTED_EDGE('',*,*,#3234,.F.);
#4364=ORIENTED_EDGE('',*,*,#3235,.F.);
#4365=ORIENTED_EDGE('',*,*,#3234,.T.);
#4366=ORIENTED_EDGE('',*,*,#3236,.F.);
#4367=ORIENTED_EDGE('',*,*,#3237,.F.);
#4368=ORIENTED_EDGE('',*,*,#3238,.F.);
#4369=ORIENTED_EDGE('',*,*,#3237,.T.);
#4370=ORIENTED_EDGE('',*,*,#3239,.F.);
#4371=ORIENTED_EDGE('',*,*,#3240,.F.);
#4372=ORIENTED_EDGE('',*,*,#3241,.F.);
#4373=ORIENTED_EDGE('',*,*,#3240,.T.);
#4374=ORIENTED_EDGE('',*,*,#3242,.F.);
#4375=ORIENTED_EDGE('',*,*,#3243,.F.);
#4376=ORIENTED_EDGE('',*,*,#3244,.F.);
#4377=ORIENTED_EDGE('',*,*,#3243,.T.);
#4378=ORIENTED_EDGE('',*,*,#3245,.F.);
#4379=ORIENTED_EDGE('',*,*,#3223,.F.);
#4380=ORIENTED_EDGE('',*,*,#3244,.T.);
#4381=ORIENTED_EDGE('',*,*,#3222,.T.);
#4382=ORIENTED_EDGE('',*,*,#3226,.T.);
#4383=ORIENTED_EDGE('',*,*,#3229,.T.);
#4384=ORIENTED_EDGE('',*,*,#3232,.T.);
#4385=ORIENTED_EDGE('',*,*,#3235,.T.);
#4386=ORIENTED_EDGE('',*,*,#3238,.T.);
#4387=ORIENTED_EDGE('',*,*,#3241,.T.);
#4388=ORIENTED_EDGE('',*,*,#3245,.T.);
#4389=ORIENTED_EDGE('',*,*,#3242,.T.);
#4390=ORIENTED_EDGE('',*,*,#3239,.T.);
#4391=ORIENTED_EDGE('',*,*,#3236,.T.);
#4392=ORIENTED_EDGE('',*,*,#3233,.T.);
#4393=ORIENTED_EDGE('',*,*,#3230,.T.);
#4394=ORIENTED_EDGE('',*,*,#3227,.T.);
#4395=ORIENTED_EDGE('',*,*,#3224,.T.);
#4396=ORIENTED_EDGE('',*,*,#3246,.F.);
#4397=ORIENTED_EDGE('',*,*,#3247,.T.);
#4398=ORIENTED_EDGE('',*,*,#3248,.F.);
#4399=ORIENTED_EDGE('',*,*,#3247,.F.);
#4400=ORIENTED_EDGE('',*,*,#3249,.F.);
#4401=ORIENTED_EDGE('',*,*,#3250,.T.);
#4402=ORIENTED_EDGE('',*,*,#3251,.F.);
#4403=ORIENTED_EDGE('',*,*,#3250,.F.);
#4404=ORIENTED_EDGE('',*,*,#3252,.F.);
#4405=ORIENTED_EDGE('',*,*,#3253,.T.);
#4406=ORIENTED_EDGE('',*,*,#3254,.F.);
#4407=ORIENTED_EDGE('',*,*,#3253,.F.);
#4408=ORIENTED_EDGE('',*,*,#3255,.F.);
#4409=ORIENTED_EDGE('',*,*,#3256,.T.);
#4410=ORIENTED_EDGE('',*,*,#3257,.F.);
#4411=ORIENTED_EDGE('',*,*,#3256,.F.);
#4412=ORIENTED_EDGE('',*,*,#3258,.F.);
#4413=ORIENTED_EDGE('',*,*,#3259,.T.);
#4414=ORIENTED_EDGE('',*,*,#3260,.F.);
#4415=ORIENTED_EDGE('',*,*,#3259,.F.);
#4416=ORIENTED_EDGE('',*,*,#3261,.F.);
#4417=ORIENTED_EDGE('',*,*,#3262,.T.);
#4418=ORIENTED_EDGE('',*,*,#3263,.F.);
#4419=ORIENTED_EDGE('',*,*,#3262,.F.);
#4420=ORIENTED_EDGE('',*,*,#3264,.T.);
#4421=ORIENTED_EDGE('',*,*,#3265,.T.);
#4422=ORIENTED_EDGE('',*,*,#3266,.F.);
#4423=ORIENTED_EDGE('',*,*,#3267,.F.);
#4424=ORIENTED_EDGE('',*,*,#3268,.T.);
#4425=ORIENTED_EDGE('',*,*,#3267,.T.);
#4426=ORIENTED_EDGE('',*,*,#3269,.F.);
#4427=ORIENTED_EDGE('',*,*,#3270,.F.);
#4428=ORIENTED_EDGE('',*,*,#3271,.T.);
#4429=ORIENTED_EDGE('',*,*,#3270,.T.);
#4430=ORIENTED_EDGE('',*,*,#3272,.F.);
#4431=ORIENTED_EDGE('',*,*,#3273,.F.);
#4432=ORIENTED_EDGE('',*,*,#3274,.T.);
#4433=ORIENTED_EDGE('',*,*,#3273,.T.);
#4434=ORIENTED_EDGE('',*,*,#3275,.F.);
#4435=ORIENTED_EDGE('',*,*,#3265,.F.);
#4436=ORIENTED_EDGE('',*,*,#3275,.T.);
#4437=ORIENTED_EDGE('',*,*,#3272,.T.);
#4438=ORIENTED_EDGE('',*,*,#3269,.T.);
#4439=ORIENTED_EDGE('',*,*,#3266,.T.);
#4440=ORIENTED_EDGE('',*,*,#3248,.T.);
#4441=ORIENTED_EDGE('',*,*,#3251,.T.);
#4442=ORIENTED_EDGE('',*,*,#3254,.T.);
#4443=ORIENTED_EDGE('',*,*,#3257,.T.);
#4444=ORIENTED_EDGE('',*,*,#3260,.T.);
#4445=ORIENTED_EDGE('',*,*,#3263,.T.);
#4446=ORIENTED_EDGE('',*,*,#3274,.F.);
#4447=ORIENTED_EDGE('',*,*,#3264,.F.);
#4448=ORIENTED_EDGE('',*,*,#3268,.F.);
#4449=ORIENTED_EDGE('',*,*,#3271,.F.);
#4450=ORIENTED_EDGE('',*,*,#3246,.T.);
#4451=ORIENTED_EDGE('',*,*,#3249,.T.);
#4452=ORIENTED_EDGE('',*,*,#3252,.T.);
#4453=ORIENTED_EDGE('',*,*,#3255,.T.);
#4454=ORIENTED_EDGE('',*,*,#3258,.T.);
#4455=ORIENTED_EDGE('',*,*,#3261,.T.);
#4456=ORIENTED_EDGE('',*,*,#3276,.F.);
#4457=ORIENTED_EDGE('',*,*,#3277,.T.);
#4458=ORIENTED_EDGE('',*,*,#3278,.T.);
#4459=ORIENTED_EDGE('',*,*,#3277,.F.);
#4460=ORIENTED_EDGE('',*,*,#3279,.F.);
#4461=ORIENTED_EDGE('',*,*,#3280,.T.);
#4462=ORIENTED_EDGE('',*,*,#3281,.T.);
#4463=ORIENTED_EDGE('',*,*,#3280,.F.);
#4464=ORIENTED_EDGE('',*,*,#3279,.T.);
#4465=ORIENTED_EDGE('',*,*,#3276,.T.);
#4466=ORIENTED_EDGE('',*,*,#3281,.F.);
#4467=ORIENTED_EDGE('',*,*,#3278,.F.);
#4468=ORIENTED_EDGE('',*,*,#3282,.T.);
#4469=ORIENTED_EDGE('',*,*,#3283,.T.);
#4470=ORIENTED_EDGE('',*,*,#3284,.T.);
#4471=ORIENTED_EDGE('',*,*,#3283,.F.);
#4472=ORIENTED_EDGE('',*,*,#3284,.F.);
#4473=ORIENTED_EDGE('',*,*,#3285,.T.);
#4474=ORIENTED_EDGE('',*,*,#3286,.T.);
#4475=ORIENTED_EDGE('',*,*,#3285,.F.);
#4476=ORIENTED_EDGE('',*,*,#3287,.T.);
#4477=ORIENTED_EDGE('',*,*,#3282,.F.);
#4478=ORIENTED_EDGE('',*,*,#3287,.F.);
#4479=ORIENTED_EDGE('',*,*,#3288,.T.);
#4480=ORIENTED_EDGE('',*,*,#3289,.T.);
#4481=ORIENTED_EDGE('',*,*,#3288,.F.);
#4482=ORIENTED_EDGE('',*,*,#3289,.F.);
#4483=ORIENTED_EDGE('',*,*,#3286,.F.);
#4484=ORIENTED_EDGE('',*,*,#3290,.F.);
#4485=ORIENTED_EDGE('',*,*,#3291,.F.);
#4486=ORIENTED_EDGE('',*,*,#3292,.T.);
#4487=ORIENTED_EDGE('',*,*,#3290,.T.);
#4488=ORIENTED_EDGE('',*,*,#3292,.F.);
#4489=ORIENTED_EDGE('',*,*,#3293,.F.);
#4490=ORIENTED_EDGE('',*,*,#3294,.T.);
#4491=ORIENTED_EDGE('',*,*,#3291,.T.);
#4492=ORIENTED_EDGE('',*,*,#3294,.F.);
#4493=ORIENTED_EDGE('',*,*,#3295,.F.);
#4494=ORIENTED_EDGE('',*,*,#3296,.T.);
#4495=ORIENTED_EDGE('',*,*,#3293,.T.);
#4496=ORIENTED_EDGE('',*,*,#3296,.F.);
#4497=ORIENTED_EDGE('',*,*,#3295,.T.);
#4498=ORIENTED_EDGE('',*,*,#3297,.F.);
#4499=ORIENTED_EDGE('',*,*,#3298,.F.);
#4500=ORIENTED_EDGE('',*,*,#3299,.T.);
#4501=ORIENTED_EDGE('',*,*,#3297,.T.);
#4502=ORIENTED_EDGE('',*,*,#3299,.F.);
#4503=ORIENTED_EDGE('',*,*,#3300,.F.);
#4504=ORIENTED_EDGE('',*,*,#3301,.T.);
#4505=ORIENTED_EDGE('',*,*,#3298,.T.);
#4506=ORIENTED_EDGE('',*,*,#3301,.F.);
#4507=ORIENTED_EDGE('',*,*,#3302,.F.);
#4508=ORIENTED_EDGE('',*,*,#3303,.T.);
#4509=ORIENTED_EDGE('',*,*,#3300,.T.);
#4510=ORIENTED_EDGE('',*,*,#3303,.F.);
#4511=ORIENTED_EDGE('',*,*,#3302,.T.);
#4512=ORIENTED_EDGE('',*,*,#3304,.T.);
#4513=ORIENTED_EDGE('',*,*,#3305,.T.);
#4514=ORIENTED_EDGE('',*,*,#3306,.T.);
#4515=ORIENTED_EDGE('',*,*,#3307,.F.);
#4516=ORIENTED_EDGE('',*,*,#3308,.T.);
#4517=ORIENTED_EDGE('',*,*,#3309,.T.);
#4518=ORIENTED_EDGE('',*,*,#3310,.T.);
#4519=ORIENTED_EDGE('',*,*,#3305,.F.);
#4520=ORIENTED_EDGE('',*,*,#3311,.T.);
#4521=ORIENTED_EDGE('',*,*,#3312,.T.);
#4522=ORIENTED_EDGE('',*,*,#3313,.T.);
#4523=ORIENTED_EDGE('',*,*,#3309,.F.);
#4524=ORIENTED_EDGE('',*,*,#3314,.T.);
#4525=ORIENTED_EDGE('',*,*,#3315,.T.);
#4526=ORIENTED_EDGE('',*,*,#3316,.T.);
#4527=ORIENTED_EDGE('',*,*,#3312,.F.);
#4528=ORIENTED_EDGE('',*,*,#3317,.T.);
#4529=ORIENTED_EDGE('',*,*,#3318,.T.);
#4530=ORIENTED_EDGE('',*,*,#3319,.T.);
#4531=ORIENTED_EDGE('',*,*,#3315,.F.);
#4532=ORIENTED_EDGE('',*,*,#3320,.T.);
#4533=ORIENTED_EDGE('',*,*,#3307,.T.);
#4534=ORIENTED_EDGE('',*,*,#3321,.T.);
#4535=ORIENTED_EDGE('',*,*,#3318,.F.);
#4536=ORIENTED_EDGE('',*,*,#3320,.F.);
#4537=ORIENTED_EDGE('',*,*,#3317,.F.);
#4538=ORIENTED_EDGE('',*,*,#3314,.F.);
#4539=ORIENTED_EDGE('',*,*,#3311,.F.);
#4540=ORIENTED_EDGE('',*,*,#3308,.F.);
#4541=ORIENTED_EDGE('',*,*,#3304,.F.);
#4542=ORIENTED_EDGE('',*,*,#3321,.F.);
#4543=ORIENTED_EDGE('',*,*,#3306,.F.);
#4544=ORIENTED_EDGE('',*,*,#3310,.F.);
#4545=ORIENTED_EDGE('',*,*,#3313,.F.);
#4546=ORIENTED_EDGE('',*,*,#3316,.F.);
#4547=ORIENTED_EDGE('',*,*,#3319,.F.);
#4548=ORIENTED_EDGE('',*,*,#3322,.F.);
#4549=ORIENTED_EDGE('',*,*,#3323,.T.);
#4550=ORIENTED_EDGE('',*,*,#3324,.T.);
#4551=ORIENTED_EDGE('',*,*,#3323,.F.);
#4552=ORIENTED_EDGE('',*,*,#3325,.F.);
#4553=ORIENTED_EDGE('',*,*,#3326,.T.);
#4554=ORIENTED_EDGE('',*,*,#3327,.T.);
#4555=ORIENTED_EDGE('',*,*,#3326,.F.);
#4556=ORIENTED_EDGE('',*,*,#3325,.T.);
#4557=ORIENTED_EDGE('',*,*,#3322,.T.);
#4558=ORIENTED_EDGE('',*,*,#3327,.F.);
#4559=ORIENTED_EDGE('',*,*,#3324,.F.);
#4560=ORIENTED_EDGE('',*,*,#3328,.F.);
#4561=ORIENTED_EDGE('',*,*,#3329,.F.);
#4562=ORIENTED_EDGE('',*,*,#3330,.T.);
#4563=ORIENTED_EDGE('',*,*,#3328,.T.);
#4564=ORIENTED_EDGE('',*,*,#3330,.F.);
#4565=ORIENTED_EDGE('',*,*,#3331,.F.);
#4566=ORIENTED_EDGE('',*,*,#3332,.T.);
#4567=ORIENTED_EDGE('',*,*,#3329,.T.);
#4568=ORIENTED_EDGE('',*,*,#3332,.F.);
#4569=ORIENTED_EDGE('',*,*,#3333,.F.);
#4570=ORIENTED_EDGE('',*,*,#3334,.T.);
#4571=ORIENTED_EDGE('',*,*,#3331,.T.);
#4572=ORIENTED_EDGE('',*,*,#3334,.F.);
#4573=ORIENTED_EDGE('',*,*,#3333,.T.);
#4574=ORIENTED_EDGE('',*,*,#3335,.F.);
#4575=ORIENTED_EDGE('',*,*,#3336,.F.);
#4576=ORIENTED_EDGE('',*,*,#3337,.T.);
#4577=ORIENTED_EDGE('',*,*,#3335,.T.);
#4578=ORIENTED_EDGE('',*,*,#3337,.F.);
#4579=ORIENTED_EDGE('',*,*,#3338,.F.);
#4580=ORIENTED_EDGE('',*,*,#3339,.T.);
#4581=ORIENTED_EDGE('',*,*,#3336,.T.);
#4582=ORIENTED_EDGE('',*,*,#3339,.F.);
#4583=ORIENTED_EDGE('',*,*,#3340,.F.);
#4584=ORIENTED_EDGE('',*,*,#3341,.T.);
#4585=ORIENTED_EDGE('',*,*,#3338,.T.);
#4586=ORIENTED_EDGE('',*,*,#3341,.F.);
#4587=ORIENTED_EDGE('',*,*,#3340,.T.);
#4588=ORIENTED_EDGE('',*,*,#3342,.T.);
#4589=ORIENTED_EDGE('',*,*,#3343,.T.);
#4590=ORIENTED_EDGE('',*,*,#3344,.T.);
#4591=ORIENTED_EDGE('',*,*,#3345,.F.);
#4592=ORIENTED_EDGE('',*,*,#3346,.T.);
#4593=ORIENTED_EDGE('',*,*,#3347,.T.);
#4594=ORIENTED_EDGE('',*,*,#3348,.T.);
#4595=ORIENTED_EDGE('',*,*,#3343,.F.);
#4596=ORIENTED_EDGE('',*,*,#3349,.T.);
#4597=ORIENTED_EDGE('',*,*,#3350,.T.);
#4598=ORIENTED_EDGE('',*,*,#3351,.T.);
#4599=ORIENTED_EDGE('',*,*,#3347,.F.);
#4600=ORIENTED_EDGE('',*,*,#3352,.T.);
#4601=ORIENTED_EDGE('',*,*,#3353,.T.);
#4602=ORIENTED_EDGE('',*,*,#3354,.T.);
#4603=ORIENTED_EDGE('',*,*,#3350,.F.);
#4604=ORIENTED_EDGE('',*,*,#3355,.T.);
#4605=ORIENTED_EDGE('',*,*,#3356,.T.);
#4606=ORIENTED_EDGE('',*,*,#3357,.T.);
#4607=ORIENTED_EDGE('',*,*,#3353,.F.);
#4608=ORIENTED_EDGE('',*,*,#3358,.T.);
#4609=ORIENTED_EDGE('',*,*,#3345,.T.);
#4610=ORIENTED_EDGE('',*,*,#3359,.T.);
#4611=ORIENTED_EDGE('',*,*,#3356,.F.);
#4612=ORIENTED_EDGE('',*,*,#3358,.F.);
#4613=ORIENTED_EDGE('',*,*,#3355,.F.);
#4614=ORIENTED_EDGE('',*,*,#3352,.F.);
#4615=ORIENTED_EDGE('',*,*,#3349,.F.);
#4616=ORIENTED_EDGE('',*,*,#3346,.F.);
#4617=ORIENTED_EDGE('',*,*,#3342,.F.);
#4618=ORIENTED_EDGE('',*,*,#3359,.F.);
#4619=ORIENTED_EDGE('',*,*,#3344,.F.);
#4620=ORIENTED_EDGE('',*,*,#3348,.F.);
#4621=ORIENTED_EDGE('',*,*,#3351,.F.);
#4622=ORIENTED_EDGE('',*,*,#3354,.F.);
#4623=ORIENTED_EDGE('',*,*,#3357,.F.);
#4624=CYLINDRICAL_SURFACE('',#5165,0.165);
#4625=CYLINDRICAL_SURFACE('',#5168,0.164999999999999);
#4626=CYLINDRICAL_SURFACE('',#5171,0.210000000000001);
#4627=CYLINDRICAL_SURFACE('',#5174,0.21);
#4628=CYLINDRICAL_SURFACE('',#5177,0.21);
#4629=CYLINDRICAL_SURFACE('',#5180,0.210000000000001);
#4630=CYLINDRICAL_SURFACE('',#5183,0.274999999999999);
#4631=CYLINDRICAL_SURFACE('',#5186,0.275);
#4632=CYLINDRICAL_SURFACE('',#5189,0.275);
#4633=CYLINDRICAL_SURFACE('',#5192,0.274999999999999);
#4634=CYLINDRICAL_SURFACE('',#5195,0.164999999999999);
#4635=CYLINDRICAL_SURFACE('',#5198,0.164999999999999);
#4636=CYLINDRICAL_SURFACE('',#5201,0.165);
#4637=CYLINDRICAL_SURFACE('',#5204,0.164999999999999);
#4638=CYLINDRICAL_SURFACE('',#5250,0.21);
#4639=CYLINDRICAL_SURFACE('',#5275,0.2117);
#4640=CYLINDRICAL_SURFACE('',#5299,0.425);
#4641=CYLINDRICAL_SURFACE('',#5307,0.24505);
#4642=CYLINDRICAL_SURFACE('',#5309,0.375);
#4643=CYLINDRICAL_SURFACE('',#5314,0.375);
#4644=CYLINDRICAL_SURFACE('',#5319,0.375);
#4645=CYLINDRICAL_SURFACE('',#5324,0.375);
#4646=CYLINDRICAL_SURFACE('',#5329,0.225);
#4647=CYLINDRICAL_SURFACE('',#5331,0.225);
#4648=CYLINDRICAL_SURFACE('',#5333,0.225);
#4649=CYLINDRICAL_SURFACE('',#5335,0.225000000000001);
#4650=CYLINDRICAL_SURFACE('',#5356,0.35);
#4651=CYLINDRICAL_SURFACE('',#5364,0.1954);
#4652=CYLINDRICAL_SURFACE('',#5378,0.475);
#4653=CYLINDRICAL_SURFACE('',#5383,0.475);
#4654=CYLINDRICAL_SURFACE('',#5388,0.275);
#4655=CYLINDRICAL_SURFACE('',#5390,0.275);
#4656=CYLINDRICAL_SURFACE('',#5417,0.21);
#4657=CYLINDRICAL_SURFACE('',#5423,0.21);
#4658=CYLINDRICAL_SURFACE('',#5429,0.21);
#4659=CYLINDRICAL_SURFACE('',#5435,0.21);
#4660=CYLINDRICAL_SURFACE('',#5479,0.164999999999999);
#4661=CYLINDRICAL_SURFACE('',#5482,0.25);
#4662=CYLINDRICAL_SURFACE('',#5485,0.275);
#4663=CYLINDRICAL_SURFACE('',#5488,0.275);
#4664=CYLINDRICAL_SURFACE('',#5491,0.275);
#4665=CYLINDRICAL_SURFACE('',#5494,0.275);
#4666=CYLINDRICAL_SURFACE('',#5504,0.33);
#4667=CYLINDRICAL_SURFACE('',#5507,1.5);
#4668=CYLINDRICAL_SURFACE('',#5516,0.265);
#4669=CYLINDRICAL_SURFACE('',#5520,0.5);
#4670=CYLINDRICAL_SURFACE('',#5528,0.425);
#4671=CYLINDRICAL_SURFACE('',#5536,0.24505);
#4672=CYLINDRICAL_SURFACE('',#5582,0.32);
#4673=CYLINDRICAL_SURFACE('',#5585,0.6);
#4674=CYLINDRICAL_SURFACE('',#5595,0.5);
#4675=CYLINDRICAL_SURFACE('',#5603,0.2942);
#4676=ADVANCED_FACE('',(#577),#4624,.F.);
#4677=ADVANCED_FACE('',(#578),#4625,.F.);
#4678=ADVANCED_FACE('',(#579),#4626,.F.);
#4679=ADVANCED_FACE('',(#580),#4627,.F.);
#4680=ADVANCED_FACE('',(#581),#4628,.F.);
#4681=ADVANCED_FACE('',(#582),#4629,.F.);
#4682=ADVANCED_FACE('',(#583),#4630,.F.);
#4683=ADVANCED_FACE('',(#584),#4631,.F.);
#4684=ADVANCED_FACE('',(#585),#4632,.F.);
#4685=ADVANCED_FACE('',(#586),#4633,.F.);
#4686=ADVANCED_FACE('',(#587),#4634,.F.);
#4687=ADVANCED_FACE('',(#588),#4635,.F.);
#4688=ADVANCED_FACE('',(#589),#4636,.F.);
#4689=ADVANCED_FACE('',(#590),#4637,.F.);
#4690=ADVANCED_FACE('',(#591),#380,.T.);
#4691=ADVANCED_FACE('',(#592),#381,.T.);
#4692=ADVANCED_FACE('',(#593),#382,.T.);
#4693=ADVANCED_FACE('',(#594),#383,.T.);
#4694=ADVANCED_FACE('',(#595,#305,#306,#307,#308,#309,#310,#311,#312,#313,
#314,#315,#316,#317,#318),#384,.T.);
#4695=ADVANCED_FACE('',(#596,#319,#320,#321,#322,#323,#324,#325,#326,#327,
#328,#329,#330,#331,#332),#385,.F.);
#4696=ADVANCED_FACE('',(#597),#386,.F.);
#4697=ADVANCED_FACE('',(#598),#387,.F.);
#4698=ADVANCED_FACE('',(#599),#388,.F.);
#4699=ADVANCED_FACE('',(#600),#389,.F.);
#4700=ADVANCED_FACE('',(#601),#390,.F.);
#4701=ADVANCED_FACE('',(#602),#391,.F.);
#4702=ADVANCED_FACE('',(#603),#392,.F.);
#4703=ADVANCED_FACE('',(#604),#393,.F.);
#4704=ADVANCED_FACE('',(#605),#394,.F.);
#4705=ADVANCED_FACE('',(#606),#395,.F.);
#4706=ADVANCED_FACE('',(#607),#396,.F.);
#4707=ADVANCED_FACE('',(#608),#397,.F.);
#4708=ADVANCED_FACE('',(#609),#398,.F.);
#4709=ADVANCED_FACE('',(#610),#399,.F.);
#4710=ADVANCED_FACE('',(#611),#400,.F.);
#4711=ADVANCED_FACE('',(#612),#401,.F.);
#4712=ADVANCED_FACE('',(#613),#402,.F.);
#4713=ADVANCED_FACE('',(#614),#403,.F.);
#4714=ADVANCED_FACE('',(#615),#404,.F.);
#4715=ADVANCED_FACE('',(#616),#405,.F.);
#4716=ADVANCED_FACE('',(#617),#406,.F.);
#4717=ADVANCED_FACE('',(#618),#407,.F.);
#4718=ADVANCED_FACE('',(#619),#408,.F.);
#4719=ADVANCED_FACE('',(#620),#409,.F.);
#4720=ADVANCED_FACE('',(#621),#410,.F.);
#4721=ADVANCED_FACE('',(#622),#411,.F.);
#4722=ADVANCED_FACE('',(#623),#412,.F.);
#4723=ADVANCED_FACE('',(#624),#413,.F.);
#4724=ADVANCED_FACE('',(#625),#414,.F.);
#4725=ADVANCED_FACE('',(#626),#415,.F.);
#4726=ADVANCED_FACE('',(#627),#416,.F.);
#4727=ADVANCED_FACE('',(#628),#417,.F.);
#4728=ADVANCED_FACE('',(#629),#418,.F.);
#4729=ADVANCED_FACE('',(#630),#419,.F.);
#4730=ADVANCED_FACE('',(#631),#420,.F.);
#4731=ADVANCED_FACE('',(#632),#421,.F.);
#4732=ADVANCED_FACE('',(#633),#4638,.F.);
#4733=ADVANCED_FACE('',(#634),#422,.T.);
#4734=ADVANCED_FACE('',(#635),#423,.T.);
#4735=ADVANCED_FACE('',(#636),#424,.T.);
#4736=ADVANCED_FACE('',(#637),#425,.T.);
#4737=ADVANCED_FACE('',(#638),#426,.T.);
#4738=ADVANCED_FACE('',(#639),#427,.T.);
#4739=ADVANCED_FACE('',(#640),#428,.T.);
#4740=ADVANCED_FACE('',(#641),#429,.T.);
#4741=ADVANCED_FACE('',(#642,#333),#430,.T.);
#4742=ADVANCED_FACE('',(#643,#334),#431,.F.);
#4743=ADVANCED_FACE('',(#644),#432,.F.);
#4744=ADVANCED_FACE('',(#645),#433,.T.);
#4745=ADVANCED_FACE('',(#646,#335),#434,.T.);
#4746=ADVANCED_FACE('',(#647),#435,.T.);
#4747=ADVANCED_FACE('',(#648),#436,.T.);
#4748=ADVANCED_FACE('',(#649),#437,.F.);
#4749=ADVANCED_FACE('',(#650),#438,.T.);
#4750=ADVANCED_FACE('',(#651),#439,.T.);
#4751=ADVANCED_FACE('',(#652),#440,.T.);
#4752=ADVANCED_FACE('',(#653),#4639,.F.);
#4753=ADVANCED_FACE('',(#654),#441,.F.);
#4754=ADVANCED_FACE('',(#655),#442,.F.);
#4755=ADVANCED_FACE('',(#656),#443,.T.);
#4756=ADVANCED_FACE('',(#657),#444,.T.);
#4757=ADVANCED_FACE('',(#658),#445,.F.);
#4758=ADVANCED_FACE('',(#659),#446,.F.);
#4759=ADVANCED_FACE('',(#660),#447,.F.);
#4760=ADVANCED_FACE('',(#661),#448,.F.);
#4761=ADVANCED_FACE('',(#662),#449,.F.);
#4762=ADVANCED_FACE('',(#663),#450,.F.);
#4763=ADVANCED_FACE('',(#664),#451,.F.);
#4764=ADVANCED_FACE('',(#665),#452,.F.);
#4765=ADVANCED_FACE('',(#666),#453,.F.);
#4766=ADVANCED_FACE('',(#667),#454,.T.);
#4767=ADVANCED_FACE('',(#668),#211,.T.);
#4768=ADVANCED_FACE('',(#669),#4640,.T.);
#4769=ADVANCED_FACE('',(#670),#212,.T.);
#4770=ADVANCED_FACE('',(#671,#336),#455,.T.);
#4771=ADVANCED_FACE('',(#672),#213,.T.);
#4772=ADVANCED_FACE('',(#673),#4641,.T.);
#4773=ADVANCED_FACE('',(#674),#4642,.F.);
#4774=ADVANCED_FACE('',(#675,#337),#456,.T.);
#4775=ADVANCED_FACE('',(#676),#4643,.F.);
#4776=ADVANCED_FACE('',(#677,#338),#457,.T.);
#4777=ADVANCED_FACE('',(#678),#4644,.F.);
#4778=ADVANCED_FACE('',(#679,#339),#458,.T.);
#4779=ADVANCED_FACE('',(#680),#4645,.F.);
#4780=ADVANCED_FACE('',(#681,#340),#459,.T.);
#4781=ADVANCED_FACE('',(#682),#4646,.F.);
#4782=ADVANCED_FACE('',(#683),#4647,.F.);
#4783=ADVANCED_FACE('',(#684),#4648,.F.);
#4784=ADVANCED_FACE('',(#685),#4649,.F.);
#4785=ADVANCED_FACE('',(#686),#460,.T.);
#4786=ADVANCED_FACE('',(#687),#461,.T.);
#4787=ADVANCED_FACE('',(#688),#462,.T.);
#4788=ADVANCED_FACE('',(#689),#463,.T.);
#4789=ADVANCED_FACE('',(#690,#341,#342,#343,#344),#464,.T.);
#4790=ADVANCED_FACE('',(#691),#465,.T.);
#4791=ADVANCED_FACE('',(#692),#466,.T.);
#4792=ADVANCED_FACE('',(#693),#467,.T.);
#4793=ADVANCED_FACE('',(#694),#468,.T.);
#4794=ADVANCED_FACE('',(#695),#469,.T.);
#4795=ADVANCED_FACE('',(#696,#345,#346,#347,#348),#470,.T.);
#4796=ADVANCED_FACE('',(#697),#471,.T.);
#4797=ADVANCED_FACE('',(#698),#472,.T.);
#4798=ADVANCED_FACE('',(#699),#473,.F.);
#4799=ADVANCED_FACE('',(#700),#474,.T.);
#4800=ADVANCED_FACE('',(#701),#214,.T.);
#4801=ADVANCED_FACE('',(#702),#4650,.T.);
#4802=ADVANCED_FACE('',(#703),#215,.T.);
#4803=ADVANCED_FACE('',(#704,#349),#475,.T.);
#4804=ADVANCED_FACE('',(#705),#216,.T.);
#4805=ADVANCED_FACE('',(#706),#4651,.T.);
#4806=ADVANCED_FACE('',(#707),#217,.T.);
#4807=ADVANCED_FACE('',(#708),#476,.T.);
#4808=ADVANCED_FACE('',(#709),#477,.F.);
#4809=ADVANCED_FACE('',(#710),#478,.F.);
#4810=ADVANCED_FACE('',(#711),#479,.F.);
#4811=ADVANCED_FACE('',(#712),#480,.F.);
#4812=ADVANCED_FACE('',(#713),#481,.F.);
#4813=ADVANCED_FACE('',(#714),#482,.F.);
#4814=ADVANCED_FACE('',(#715),#483,.F.);
#4815=ADVANCED_FACE('',(#716),#484,.F.);
#4816=ADVANCED_FACE('',(#717),#4652,.F.);
#4817=ADVANCED_FACE('',(#718,#350),#485,.T.);
#4818=ADVANCED_FACE('',(#719),#4653,.F.);
#4819=ADVANCED_FACE('',(#720,#351),#486,.T.);
#4820=ADVANCED_FACE('',(#721),#4654,.F.);
#4821=ADVANCED_FACE('',(#722),#4655,.F.);
#4822=ADVANCED_FACE('',(#723),#487,.T.);
#4823=ADVANCED_FACE('',(#724),#488,.T.);
#4824=ADVANCED_FACE('',(#725),#489,.T.);
#4825=ADVANCED_FACE('',(#726),#490,.T.);
#4826=ADVANCED_FACE('',(#727,#352,#353),#491,.T.);
#4827=ADVANCED_FACE('',(#728,#354,#355),#492,.F.);
#4828=ADVANCED_FACE('',(#729),#493,.T.);
#4829=ADVANCED_FACE('',(#730),#494,.T.);
#4830=ADVANCED_FACE('',(#731),#495,.T.);
#4831=ADVANCED_FACE('',(#732),#496,.T.);
#4832=ADVANCED_FACE('',(#733),#497,.T.);
#4833=ADVANCED_FACE('',(#734),#498,.F.);
#4834=ADVANCED_FACE('',(#735),#499,.T.);
#4835=ADVANCED_FACE('',(#736),#500,.T.);
#4836=ADVANCED_FACE('',(#737),#501,.T.);
#4837=ADVANCED_FACE('',(#738),#502,.T.);
#4838=ADVANCED_FACE('',(#739),#503,.T.);
#4839=ADVANCED_FACE('',(#740),#504,.F.);
#4840=ADVANCED_FACE('',(#741),#505,.T.);
#4841=ADVANCED_FACE('',(#742),#4656,.F.);
#4842=ADVANCED_FACE('',(#743),#506,.T.);
#4843=ADVANCED_FACE('',(#744),#4657,.F.);
#4844=ADVANCED_FACE('',(#745),#507,.T.);
#4845=ADVANCED_FACE('',(#746),#4658,.F.);
#4846=ADVANCED_FACE('',(#747),#508,.T.);
#4847=ADVANCED_FACE('',(#748),#4659,.F.);
#4848=ADVANCED_FACE('',(#749),#509,.T.);
#4849=ADVANCED_FACE('',(#750),#510,.T.);
#4850=ADVANCED_FACE('',(#751),#511,.T.);
#4851=ADVANCED_FACE('',(#752),#512,.T.);
#4852=ADVANCED_FACE('',(#753),#513,.T.);
#4853=ADVANCED_FACE('',(#754,#356,#357,#358,#359),#514,.T.);
#4854=ADVANCED_FACE('',(#755),#515,.T.);
#4855=ADVANCED_FACE('',(#756),#516,.T.);
#4856=ADVANCED_FACE('',(#757),#517,.T.);
#4857=ADVANCED_FACE('',(#758),#518,.T.);
#4858=ADVANCED_FACE('',(#759),#519,.T.);
#4859=ADVANCED_FACE('',(#760),#520,.T.);
#4860=ADVANCED_FACE('',(#761),#521,.T.);
#4861=ADVANCED_FACE('',(#762),#522,.T.);
#4862=ADVANCED_FACE('',(#763),#523,.T.);
#4863=ADVANCED_FACE('',(#764),#524,.T.);
#4864=ADVANCED_FACE('',(#765),#525,.T.);
#4865=ADVANCED_FACE('',(#766),#526,.T.);
#4866=ADVANCED_FACE('',(#767),#527,.T.);
#4867=ADVANCED_FACE('',(#768),#528,.T.);
#4868=ADVANCED_FACE('',(#769),#529,.T.);
#4869=ADVANCED_FACE('',(#770),#530,.T.);
#4870=ADVANCED_FACE('',(#771),#531,.T.);
#4871=ADVANCED_FACE('',(#772),#532,.F.);
#4872=ADVANCED_FACE('',(#773),#533,.T.);
#4873=ADVANCED_FACE('',(#774),#534,.T.);
#4874=ADVANCED_FACE('',(#775),#535,.T.);
#4875=ADVANCED_FACE('',(#776),#536,.T.);
#4876=ADVANCED_FACE('',(#777),#537,.T.);
#4877=ADVANCED_FACE('',(#778),#538,.T.);
#4878=ADVANCED_FACE('',(#779),#539,.T.);
#4879=ADVANCED_FACE('',(#780),#540,.T.);
#4880=ADVANCED_FACE('',(#781),#541,.T.);
#4881=ADVANCED_FACE('',(#782),#542,.T.);
#4882=ADVANCED_FACE('',(#783),#4660,.F.);
#4883=ADVANCED_FACE('',(#784),#4661,.F.);
#4884=ADVANCED_FACE('',(#785),#4662,.F.);
#4885=ADVANCED_FACE('',(#786),#4663,.F.);
#4886=ADVANCED_FACE('',(#787),#4664,.F.);
#4887=ADVANCED_FACE('',(#788),#4665,.F.);
#4888=ADVANCED_FACE('',(#789),#543,.T.);
#4889=ADVANCED_FACE('',(#790),#544,.T.);
#4890=ADVANCED_FACE('',(#791),#545,.T.);
#4891=ADVANCED_FACE('',(#792),#546,.T.);
#4892=ADVANCED_FACE('',(#793,#360,#361,#362,#363,#364,#365),#547,.T.);
#4893=ADVANCED_FACE('',(#794,#366,#367,#368,#369,#370,#371),#548,.F.);
#4894=ADVANCED_FACE('',(#795),#4666,.F.);
#4895=ADVANCED_FACE('',(#796),#4667,.T.);
#4896=ADVANCED_FACE('',(#797,#372),#549,.T.);
#4897=ADVANCED_FACE('',(#798,#373),#550,.F.);
#4898=ADVANCED_FACE('',(#799),#218,.F.);
#4899=ADVANCED_FACE('',(#800),#4668,.F.);
#4900=ADVANCED_FACE('',(#801,#374),#551,.T.);
#4901=ADVANCED_FACE('',(#802),#4669,.T.);
#4902=ADVANCED_FACE('',(#803,#375),#552,.F.);
#4903=ADVANCED_FACE('',(#804),#553,.T.);
#4904=ADVANCED_FACE('',(#805),#219,.T.);
#4905=ADVANCED_FACE('',(#806),#4670,.T.);
#4906=ADVANCED_FACE('',(#807),#220,.T.);
#4907=ADVANCED_FACE('',(#808,#376),#554,.T.);
#4908=ADVANCED_FACE('',(#809),#221,.T.);
#4909=ADVANCED_FACE('',(#810),#4671,.T.);
#4910=ADVANCED_FACE('',(#811),#222,.T.);
#4911=ADVANCED_FACE('',(#812),#555,.T.);
#4912=ADVANCED_FACE('',(#813),#556,.F.);
#4913=ADVANCED_FACE('',(#814),#557,.F.);
#4914=ADVANCED_FACE('',(#815),#558,.F.);
#4915=ADVANCED_FACE('',(#816),#559,.F.);
#4916=ADVANCED_FACE('',(#817),#560,.F.);
#4917=ADVANCED_FACE('',(#818),#561,.F.);
#4918=ADVANCED_FACE('',(#819),#562,.F.);
#4919=ADVANCED_FACE('',(#820),#563,.F.);
#4920=ADVANCED_FACE('',(#821),#4672,.F.);
#4921=ADVANCED_FACE('',(#822),#4673,.T.);
#4922=ADVANCED_FACE('',(#823,#377),#564,.T.);
#4923=ADVANCED_FACE('',(#824,#378),#565,.F.);
#4924=ADVANCED_FACE('',(#825),#566,.T.);
#4925=ADVANCED_FACE('',(#826),#223,.T.);
#4926=ADVANCED_FACE('',(#827),#4674,.T.);
#4927=ADVANCED_FACE('',(#828),#224,.T.);
#4928=ADVANCED_FACE('',(#829,#379),#567,.T.);
#4929=ADVANCED_FACE('',(#830),#225,.T.);
#4930=ADVANCED_FACE('',(#831),#4675,.T.);
#4931=ADVANCED_FACE('',(#832),#226,.T.);
#4932=ADVANCED_FACE('',(#833),#568,.T.);
#4933=ADVANCED_FACE('',(#834),#569,.F.);
#4934=ADVANCED_FACE('',(#835),#570,.F.);
#4935=ADVANCED_FACE('',(#836),#571,.F.);
#4936=ADVANCED_FACE('',(#837),#572,.F.);
#4937=ADVANCED_FACE('',(#838),#573,.F.);
#4938=ADVANCED_FACE('',(#839),#574,.F.);
#4939=ADVANCED_FACE('',(#840),#575,.F.);
#4940=ADVANCED_FACE('',(#841),#576,.F.);
#4941=CLOSED_SHELL('',(#4676,#4677,#4678,#4679,#4680,#4681,#4682,#4683,
#4684,#4685,#4686,#4687,#4688,#4689,#4690,#4691,#4692,#4693,#4694,#4695));
#4942=CLOSED_SHELL('',(#4696,#4697,#4698,#4699,#4700,#4701,#4702,#4703,
#4704,#4705,#4706,#4707,#4708,#4709,#4710,#4711,#4712,#4713,#4714,#4715,
#4716,#4717,#4718,#4719,#4720,#4721,#4722,#4723,#4724,#4725,#4726,#4727,
#4728,#4729,#4730,#4731,#4732,#4733,#4734,#4735,#4736,#4737,#4738,#4739,
#4740,#4741,#4742));
#4943=CLOSED_SHELL('',(#4743,#4744,#4745,#4746,#4747,#4748,#4749,#4750,
#4751,#4752,#4753,#4754,#4755,#4756));
#4944=CLOSED_SHELL('',(#4757,#4758,#4759,#4760,#4761,#4762,#4763,#4764));
#4945=CLOSED_SHELL('',(#4765,#4766,#4767,#4768,#4769,#4770,#4771,#4772));
#4946=CLOSED_SHELL('',(#4773,#4774,#4775,#4776,#4777,#4778,#4779,#4780,
#4781,#4782,#4783,#4784,#4785,#4786,#4787,#4788,#4789,#4790,#4791,#4792,
#4793,#4794,#4795,#4796,#4797,#4798));
#4947=CLOSED_SHELL('',(#4799,#4800,#4801,#4802,#4803,#4804,#4805,#4806,
#4807));
#4948=CLOSED_SHELL('',(#4808,#4809,#4810,#4811,#4812,#4813,#4814,#4815));
#4949=CLOSED_SHELL('',(#4816,#4817,#4818,#4819,#4820,#4821,#4822,#4823,
#4824,#4825,#4826,#4827));
#4950=CLOSED_SHELL('',(#4828,#4829,#4830,#4831,#4832,#4833));
#4951=CLOSED_SHELL('',(#4834,#4835,#4836,#4837,#4838,#4839));
#4952=CLOSED_SHELL('',(#4840,#4841,#4842,#4843,#4844,#4845,#4846,#4847,
#4848,#4849,#4850,#4851,#4852,#4853,#4854,#4855,#4856,#4857,#4858,#4859,
#4860,#4861));
#4953=CLOSED_SHELL('',(#4862,#4863,#4864,#4865,#4866,#4867,#4868,#4869,
#4870,#4871));
#4954=CLOSED_SHELL('',(#4872,#4873,#4874,#4875,#4876,#4877,#4878,#4879,
#4880,#4881));
#4955=CLOSED_SHELL('',(#4882,#4883,#4884,#4885,#4886,#4887,#4888,#4889,
#4890,#4891,#4892,#4893));
#4956=CLOSED_SHELL('',(#4894,#4895,#4896,#4897));
#4957=CLOSED_SHELL('',(#4898,#4899,#4900,#4901,#4902));
#4958=CLOSED_SHELL('',(#4903,#4904,#4905,#4906,#4907,#4908,#4909,#4910,
#4911));
#4959=CLOSED_SHELL('',(#4912,#4913,#4914,#4915,#4916,#4917,#4918,#4919));
#4960=CLOSED_SHELL('',(#4920,#4921,#4922,#4923));
#4961=CLOSED_SHELL('',(#4924,#4925,#4926,#4927,#4928,#4929,#4930,#4931,
#4932));
#4962=CLOSED_SHELL('',(#4933,#4934,#4935,#4936,#4937,#4938,#4939,#4940));
#4963=DERIVED_UNIT_ELEMENT(#4999,1.);
#4964=DERIVED_UNIT_ELEMENT(#8501,-3.);
#4965=DERIVED_UNIT_ELEMENT(#4999,1.);
#4966=DERIVED_UNIT_ELEMENT(#8501,-3.);
#4967=DERIVED_UNIT_ELEMENT(#4999,1.);
#4968=DERIVED_UNIT_ELEMENT(#8501,-3.);
#4969=DERIVED_UNIT_ELEMENT(#4999,1.);
#4970=DERIVED_UNIT_ELEMENT(#8501,-3.);
#4971=DERIVED_UNIT_ELEMENT(#4999,1.);
#4972=DERIVED_UNIT_ELEMENT(#8501,-3.);
#4973=DERIVED_UNIT_ELEMENT(#4999,1.);
#4974=DERIVED_UNIT_ELEMENT(#8501,-3.);
#4975=DERIVED_UNIT_ELEMENT(#4999,1.);
#4976=DERIVED_UNIT_ELEMENT(#8501,-3.);
#4977=DERIVED_UNIT_ELEMENT(#4999,1.);
#4978=DERIVED_UNIT_ELEMENT(#8501,-3.);
#4979=DERIVED_UNIT_ELEMENT(#4999,1.);
#4980=DERIVED_UNIT_ELEMENT(#8501,-3.);
#4981=DERIVED_UNIT_ELEMENT(#4999,1.);
#4982=DERIVED_UNIT_ELEMENT(#8501,-3.);
#4983=DERIVED_UNIT_ELEMENT(#4999,1.);
#4984=DERIVED_UNIT_ELEMENT(#8501,-3.);
#4985=DERIVED_UNIT_ELEMENT(#4999,1.);
#4986=DERIVED_UNIT_ELEMENT(#8501,-3.);
#4987=DERIVED_UNIT_ELEMENT(#4999,1.);
#4988=DERIVED_UNIT_ELEMENT(#8501,-3.);
#4989=DERIVED_UNIT_ELEMENT(#4999,1.);
#4990=DERIVED_UNIT_ELEMENT(#8501,-3.);
#4991=DERIVED_UNIT_ELEMENT(#4999,1.);
#4992=DERIVED_UNIT_ELEMENT(#8501,-3.);
#4993=DERIVED_UNIT_ELEMENT(#4999,1.);
#4994=DERIVED_UNIT_ELEMENT(#8501,-3.);
#4995=DERIVED_UNIT_ELEMENT(#4999,1.);
#4996=DERIVED_UNIT_ELEMENT(#8501,-3.);
#4997=DERIVED_UNIT_ELEMENT(#4999,1.);
#4998=DERIVED_UNIT_ELEMENT(#8501,-3.);
#4999=(
MASS_UNIT()
NAMED_UNIT(*)
SI_UNIT(.KILO.,.GRAM.)
);
#5000=DERIVED_UNIT((#4963,#4964));
#5001=DERIVED_UNIT((#4965,#4966));
#5002=DERIVED_UNIT((#4967,#4968));
#5003=DERIVED_UNIT((#4969,#4970));
#5004=DERIVED_UNIT((#4971,#4972));
#5005=DERIVED_UNIT((#4973,#4974));
#5006=DERIVED_UNIT((#4975,#4976));
#5007=DERIVED_UNIT((#4977,#4978));
#5008=DERIVED_UNIT((#4979,#4980));
#5009=DERIVED_UNIT((#4981,#4982));
#5010=DERIVED_UNIT((#4983,#4984));
#5011=DERIVED_UNIT((#4985,#4986));
#5012=DERIVED_UNIT((#4987,#4988));
#5013=DERIVED_UNIT((#4989,#4990));
#5014=DERIVED_UNIT((#4991,#4992));
#5015=DERIVED_UNIT((#4993,#4994));
#5016=DERIVED_UNIT((#4995,#4996));
#5017=DERIVED_UNIT((#4997,#4998));
#5018=MEASURE_REPRESENTATION_ITEM('density measure',
POSITIVE_RATIO_MEASURE(7850.),#5000);
#5019=MEASURE_REPRESENTATION_ITEM('density measure',
POSITIVE_RATIO_MEASURE(7850.),#5001);
#5020=MEASURE_REPRESENTATION_ITEM('density measure',
POSITIVE_RATIO_MEASURE(7850.),#5002);
#5021=MEASURE_REPRESENTATION_ITEM('density measure',
POSITIVE_RATIO_MEASURE(7850.),#5003);
#5022=MEASURE_REPRESENTATION_ITEM('density measure',
POSITIVE_RATIO_MEASURE(7850.),#5004);
#5023=MEASURE_REPRESENTATION_ITEM('density measure',
POSITIVE_RATIO_MEASURE(7850.),#5005);
#5024=MEASURE_REPRESENTATION_ITEM('density measure',
POSITIVE_RATIO_MEASURE(7850.),#5006);
#5025=MEASURE_REPRESENTATION_ITEM('density measure',
POSITIVE_RATIO_MEASURE(7850.),#5007);
#5026=MEASURE_REPRESENTATION_ITEM('density measure',
POSITIVE_RATIO_MEASURE(7850.),#5008);
#5027=MEASURE_REPRESENTATION_ITEM('density measure',
POSITIVE_RATIO_MEASURE(7850.),#5009);
#5028=MEASURE_REPRESENTATION_ITEM('density measure',
POSITIVE_RATIO_MEASURE(7850.),#5010);
#5029=MEASURE_REPRESENTATION_ITEM('density measure',
POSITIVE_RATIO_MEASURE(7850.),#5011);
#5030=MEASURE_REPRESENTATION_ITEM('density measure',
POSITIVE_RATIO_MEASURE(7850.),#5012);
#5031=MEASURE_REPRESENTATION_ITEM('density measure',
POSITIVE_RATIO_MEASURE(7850.),#5013);
#5032=MEASURE_REPRESENTATION_ITEM('density measure',
POSITIVE_RATIO_MEASURE(7850.),#5014);
#5033=MEASURE_REPRESENTATION_ITEM('density measure',
POSITIVE_RATIO_MEASURE(7850.),#5015);
#5034=MEASURE_REPRESENTATION_ITEM('density measure',
POSITIVE_RATIO_MEASURE(7850.),#5016);
#5035=MEASURE_REPRESENTATION_ITEM('density measure',
POSITIVE_RATIO_MEASURE(7850.),#5017);
#5036=PROPERTY_DEFINITION_REPRESENTATION(#5126,#5072);
#5037=PROPERTY_DEFINITION_REPRESENTATION(#5127,#5073);
#5038=PROPERTY_DEFINITION_REPRESENTATION(#5128,#5074);
#5039=PROPERTY_DEFINITION_REPRESENTATION(#5129,#5075);
#5040=PROPERTY_DEFINITION_REPRESENTATION(#5130,#5076);
#5041=PROPERTY_DEFINITION_REPRESENTATION(#5131,#5077);
#5042=PROPERTY_DEFINITION_REPRESENTATION(#5132,#5078);
#5043=PROPERTY_DEFINITION_REPRESENTATION(#5133,#5079);
#5044=PROPERTY_DEFINITION_REPRESENTATION(#5134,#5080);
#5045=PROPERTY_DEFINITION_REPRESENTATION(#5135,#5081);
#5046=PROPERTY_DEFINITION_REPRESENTATION(#5136,#5082);
#5047=PROPERTY_DEFINITION_REPRESENTATION(#5137,#5083);
#5048=PROPERTY_DEFINITION_REPRESENTATION(#5138,#5084);
#5049=PROPERTY_DEFINITION_REPRESENTATION(#5139,#5085);
#5050=PROPERTY_DEFINITION_REPRESENTATION(#5140,#5086);
#5051=PROPERTY_DEFINITION_REPRESENTATION(#5141,#5087);
#5052=PROPERTY_DEFINITION_REPRESENTATION(#5142,#5088);
#5053=PROPERTY_DEFINITION_REPRESENTATION(#5143,#5089);
#5054=PROPERTY_DEFINITION_REPRESENTATION(#5144,#5090);
#5055=PROPERTY_DEFINITION_REPRESENTATION(#5145,#5091);
#5056=PROPERTY_DEFINITION_REPRESENTATION(#5146,#5092);
#5057=PROPERTY_DEFINITION_REPRESENTATION(#5147,#5093);
#5058=PROPERTY_DEFINITION_REPRESENTATION(#5148,#5094);
#5059=PROPERTY_DEFINITION_REPRESENTATION(#5149,#5095);
#5060=PROPERTY_DEFINITION_REPRESENTATION(#5150,#5096);
#5061=PROPERTY_DEFINITION_REPRESENTATION(#5151,#5097);
#5062=PROPERTY_DEFINITION_REPRESENTATION(#5152,#5098);
#5063=PROPERTY_DEFINITION_REPRESENTATION(#5153,#5099);
#5064=PROPERTY_DEFINITION_REPRESENTATION(#5154,#5100);
#5065=PROPERTY_DEFINITION_REPRESENTATION(#5155,#5101);
#5066=PROPERTY_DEFINITION_REPRESENTATION(#5156,#5102);
#5067=PROPERTY_DEFINITION_REPRESENTATION(#5157,#5103);
#5068=PROPERTY_DEFINITION_REPRESENTATION(#5158,#5104);
#5069=PROPERTY_DEFINITION_REPRESENTATION(#5159,#5105);
#5070=PROPERTY_DEFINITION_REPRESENTATION(#5160,#5106);
#5071=PROPERTY_DEFINITION_REPRESENTATION(#5161,#5107);
#5072=REPRESENTATION('material name',(#5108),#8479);
#5073=REPRESENTATION('density',(#5018),#8479);
#5074=REPRESENTATION('material name',(#5109),#8480);
#5075=REPRESENTATION('density',(#5019),#8480);
#5076=REPRESENTATION('material name',(#5110),#8481);
#5077=REPRESENTATION('density',(#5020),#8481);
#5078=REPRESENTATION('material name',(#5111),#8482);
#5079=REPRESENTATION('density',(#5021),#8482);
#5080=REPRESENTATION('material name',(#5112),#8483);
#5081=REPRESENTATION('density',(#5022),#8483);
#5082=REPRESENTATION('material name',(#5113),#8484);
#5083=REPRESENTATION('density',(#5023),#8484);
#5084=REPRESENTATION('material name',(#5114),#8485);
#5085=REPRESENTATION('density',(#5024),#8485);
#5086=REPRESENTATION('material name',(#5115),#8486);
#5087=REPRESENTATION('density',(#5025),#8486);
#5088=REPRESENTATION('material name',(#5116),#8487);
#5089=REPRESENTATION('density',(#5026),#8487);
#5090=REPRESENTATION('material name',(#5117),#8490);
#5091=REPRESENTATION('density',(#5027),#8490);
#5092=REPRESENTATION('material name',(#5118),#8491);
#5093=REPRESENTATION('density',(#5028),#8491);
#5094=REPRESENTATION('material name',(#5119),#8492);
#5095=REPRESENTATION('density',(#5029),#8492);
#5096=REPRESENTATION('material name',(#5120),#8493);
#5097=REPRESENTATION('density',(#5030),#8493);
#5098=REPRESENTATION('material name',(#5121),#8494);
#5099=REPRESENTATION('density',(#5031),#8494);
#5100=REPRESENTATION('material name',(#5122),#8495);
#5101=REPRESENTATION('density',(#5032),#8495);
#5102=REPRESENTATION('material name',(#5123),#8496);
#5103=REPRESENTATION('density',(#5033),#8496);
#5104=REPRESENTATION('material name',(#5124),#8497);
#5105=REPRESENTATION('density',(#5034),#8497);
#5106=REPRESENTATION('material name',(#5125),#8498);
#5107=REPRESENTATION('density',(#5035),#8498);
#5108=DESCRIPTIVE_REPRESENTATION_ITEM('Steel','Steel');
#5109=DESCRIPTIVE_REPRESENTATION_ITEM('Steel','Steel');
#5110=DESCRIPTIVE_REPRESENTATION_ITEM('Steel','Steel');
#5111=DESCRIPTIVE_REPRESENTATION_ITEM('Steel','Steel');
#5112=DESCRIPTIVE_REPRESENTATION_ITEM('Steel','Steel');
#5113=DESCRIPTIVE_REPRESENTATION_ITEM('Steel','Steel');
#5114=DESCRIPTIVE_REPRESENTATION_ITEM('Steel','Steel');
#5115=DESCRIPTIVE_REPRESENTATION_ITEM('Steel','Steel');
#5116=DESCRIPTIVE_REPRESENTATION_ITEM('Steel','Steel');
#5117=DESCRIPTIVE_REPRESENTATION_ITEM('Steel','Steel');
#5118=DESCRIPTIVE_REPRESENTATION_ITEM('Steel','Steel');
#5119=DESCRIPTIVE_REPRESENTATION_ITEM('Steel','Steel');
#5120=DESCRIPTIVE_REPRESENTATION_ITEM('Steel','Steel');
#5121=DESCRIPTIVE_REPRESENTATION_ITEM('Steel','Steel');
#5122=DESCRIPTIVE_REPRESENTATION_ITEM('Steel','Steel');
#5123=DESCRIPTIVE_REPRESENTATION_ITEM('Steel','Steel');
#5124=DESCRIPTIVE_REPRESENTATION_ITEM('Steel','Steel');
#5125=DESCRIPTIVE_REPRESENTATION_ITEM('Steel','Steel');
#5126=PROPERTY_DEFINITION('material property','material name',#8623);
#5127=PROPERTY_DEFINITION('material property','density of part',#8623);
#5128=PROPERTY_DEFINITION('material property','material name',#8624);
#5129=PROPERTY_DEFINITION('material property','density of part',#8624);
#5130=PROPERTY_DEFINITION('material property','material name',#8625);
#5131=PROPERTY_DEFINITION('material property','density of part',#8625);
#5132=PROPERTY_DEFINITION('material property','material name',#8626);
#5133=PROPERTY_DEFINITION('material property','density of part',#8626);
#5134=PROPERTY_DEFINITION('material property','material name',#8627);
#5135=PROPERTY_DEFINITION('material property','density of part',#8627);
#5136=PROPERTY_DEFINITION('material property','material name',#8628);
#5137=PROPERTY_DEFINITION('material property','density of part',#8628);
#5138=PROPERTY_DEFINITION('material property','material name',#8629);
#5139=PROPERTY_DEFINITION('material property','density of part',#8629);
#5140=PROPERTY_DEFINITION('material property','material name',#8630);
#5141=PROPERTY_DEFINITION('material property','density of part',#8630);
#5142=PROPERTY_DEFINITION('material property','material name',#8631);
#5143=PROPERTY_DEFINITION('material property','density of part',#8631);
#5144=PROPERTY_DEFINITION('material property','material name',#8634);
#5145=PROPERTY_DEFINITION('material property','density of part',#8634);
#5146=PROPERTY_DEFINITION('material property','material name',#8635);
#5147=PROPERTY_DEFINITION('material property','density of part',#8635);
#5148=PROPERTY_DEFINITION('material property','material name',#8636);
#5149=PROPERTY_DEFINITION('material property','density of part',#8636);
#5150=PROPERTY_DEFINITION('material property','material name',#8637);
#5151=PROPERTY_DEFINITION('material property','density of part',#8637);
#5152=PROPERTY_DEFINITION('material property','material name',#8638);
#5153=PROPERTY_DEFINITION('material property','density of part',#8638);
#5154=PROPERTY_DEFINITION('material property','material name',#8639);
#5155=PROPERTY_DEFINITION('material property','density of part',#8639);
#5156=PROPERTY_DEFINITION('material property','material name',#8640);
#5157=PROPERTY_DEFINITION('material property','density of part',#8640);
#5158=PROPERTY_DEFINITION('material property','material name',#8641);
#5159=PROPERTY_DEFINITION('material property','density of part',#8641);
#5160=PROPERTY_DEFINITION('material property','material name',#8642);
#5161=PROPERTY_DEFINITION('material property','density of part',#8642);
#5162=AXIS2_PLACEMENT_3D('',#7069,#5631,#5632);
#5163=AXIS2_PLACEMENT_3D('',#7070,#5633,#5634);
#5164=AXIS2_PLACEMENT_3D('',#7071,#5635,#5636);
#5165=AXIS2_PLACEMENT_3D('',#7072,#5637,#5638);
#5166=AXIS2_PLACEMENT_3D('',#7074,#5639,#5640);
#5167=AXIS2_PLACEMENT_3D('',#7077,#5642,#5643);
#5168=AXIS2_PLACEMENT_3D('',#7078,#5644,#5645);
#5169=AXIS2_PLACEMENT_3D('',#7080,#5646,#5647);
#5170=AXIS2_PLACEMENT_3D('',#7083,#5649,#5650);
#5171=AXIS2_PLACEMENT_3D('',#7084,#5651,#5652);
#5172=AXIS2_PLACEMENT_3D('',#7086,#5653,#5654);
#5173=AXIS2_PLACEMENT_3D('',#7089,#5656,#5657);
#5174=AXIS2_PLACEMENT_3D('',#7090,#5658,#5659);
#5175=AXIS2_PLACEMENT_3D('',#7092,#5660,#5661);
#5176=AXIS2_PLACEMENT_3D('',#7095,#5663,#5664);
#5177=AXIS2_PLACEMENT_3D('',#7096,#5665,#5666);
#5178=AXIS2_PLACEMENT_3D('',#7098,#5667,#5668);
#5179=AXIS2_PLACEMENT_3D('',#7101,#5670,#5671);
#5180=AXIS2_PLACEMENT_3D('',#7102,#5672,#5673);
#5181=AXIS2_PLACEMENT_3D('',#7104,#5674,#5675);
#5182=AXIS2_PLACEMENT_3D('',#7107,#5677,#5678);
#5183=AXIS2_PLACEMENT_3D('',#7108,#5679,#5680);
#5184=AXIS2_PLACEMENT_3D('',#7110,#5681,#5682);
#5185=AXIS2_PLACEMENT_3D('',#7113,#5684,#5685);
#5186=AXIS2_PLACEMENT_3D('',#7114,#5686,#5687);
#5187=AXIS2_PLACEMENT_3D('',#7116,#5688,#5689);
#5188=AXIS2_PLACEMENT_3D('',#7119,#5691,#5692);
#5189=AXIS2_PLACEMENT_3D('',#7120,#5693,#5694);
#5190=AXIS2_PLACEMENT_3D('',#7122,#5695,#5696);
#5191=AXIS2_PLACEMENT_3D('',#7125,#5698,#5699);
#5192=AXIS2_PLACEMENT_3D('',#7126,#5700,#5701);
#5193=AXIS2_PLACEMENT_3D('',#7128,#5702,#5703);
#5194=AXIS2_PLACEMENT_3D('',#7131,#5705,#5706);
#5195=AXIS2_PLACEMENT_3D('',#7132,#5707,#5708);
#5196=AXIS2_PLACEMENT_3D('',#7134,#5709,#5710);
#5197=AXIS2_PLACEMENT_3D('',#7137,#5712,#5713);
#5198=AXIS2_PLACEMENT_3D('',#7138,#5714,#5715);
#5199=AXIS2_PLACEMENT_3D('',#7140,#5716,#5717);
#5200=AXIS2_PLACEMENT_3D('',#7143,#5719,#5720);
#5201=AXIS2_PLACEMENT_3D('',#7144,#5721,#5722);
#5202=AXIS2_PLACEMENT_3D('',#7146,#5723,#5724);
#5203=AXIS2_PLACEMENT_3D('',#7149,#5726,#5727);
#5204=AXIS2_PLACEMENT_3D('',#7150,#5728,#5729);
#5205=AXIS2_PLACEMENT_3D('',#7152,#5730,#5731);
#5206=AXIS2_PLACEMENT_3D('',#7155,#5733,#5734);
#5207=AXIS2_PLACEMENT_3D('',#7156,#5735,#5736);
#5208=AXIS2_PLACEMENT_3D('',#7165,#5741,#5742);
#5209=AXIS2_PLACEMENT_3D('',#7171,#5746,#5747);
#5210=AXIS2_PLACEMENT_3D('',#7177,#5751,#5752);
#5211=AXIS2_PLACEMENT_3D('',#7180,#5755,#5756);
#5212=AXIS2_PLACEMENT_3D('',#7181,#5757,#5758);
#5213=AXIS2_PLACEMENT_3D('',#7182,#5759,#5760);
#5214=AXIS2_PLACEMENT_3D('',#7183,#5761,#5762);
#5215=AXIS2_PLACEMENT_3D('',#7192,#5767,#5768);
#5216=AXIS2_PLACEMENT_3D('',#7198,#5772,#5773);
#5217=AXIS2_PLACEMENT_3D('',#7204,#5777,#5778);
#5218=AXIS2_PLACEMENT_3D('',#7210,#5782,#5783);
#5219=AXIS2_PLACEMENT_3D('',#7216,#5787,#5788);
#5220=AXIS2_PLACEMENT_3D('',#7222,#5792,#5793);
#5221=AXIS2_PLACEMENT_3D('',#7228,#5797,#5798);
#5222=AXIS2_PLACEMENT_3D('',#7234,#5802,#5803);
#5223=AXIS2_PLACEMENT_3D('',#7240,#5807,#5808);
#5224=AXIS2_PLACEMENT_3D('',#7249,#5813,#5814);
#5225=AXIS2_PLACEMENT_3D('',#7255,#5818,#5819);
#5226=AXIS2_PLACEMENT_3D('',#7261,#5823,#5824);
#5227=AXIS2_PLACEMENT_3D('',#7267,#5828,#5829);
#5228=AXIS2_PLACEMENT_3D('',#7273,#5833,#5834);
#5229=AXIS2_PLACEMENT_3D('',#7279,#5838,#5839);
#5230=AXIS2_PLACEMENT_3D('',#7285,#5843,#5844);
#5231=AXIS2_PLACEMENT_3D('',#7291,#5848,#5849);
#5232=AXIS2_PLACEMENT_3D('',#7297,#5853,#5854);
#5233=AXIS2_PLACEMENT_3D('',#7306,#5859,#5860);
#5234=AXIS2_PLACEMENT_3D('',#7312,#5864,#5865);
#5235=AXIS2_PLACEMENT_3D('',#7318,#5869,#5870);
#5236=AXIS2_PLACEMENT_3D('',#7324,#5874,#5875);
#5237=AXIS2_PLACEMENT_3D('',#7330,#5879,#5880);
#5238=AXIS2_PLACEMENT_3D('',#7336,#5884,#5885);
#5239=AXIS2_PLACEMENT_3D('',#7342,#5889,#5890);
#5240=AXIS2_PLACEMENT_3D('',#7348,#5894,#5895);
#5241=AXIS2_PLACEMENT_3D('',#7354,#5899,#5900);
#5242=AXIS2_PLACEMENT_3D('',#7363,#5905,#5906);
#5243=AXIS2_PLACEMENT_3D('',#7369,#5910,#5911);
#5244=AXIS2_PLACEMENT_3D('',#7375,#5915,#5916);
#5245=AXIS2_PLACEMENT_3D('',#7381,#5920,#5921);
#5246=AXIS2_PLACEMENT_3D('',#7387,#5925,#5926);
#5247=AXIS2_PLACEMENT_3D('',#7393,#5930,#5931);
#5248=AXIS2_PLACEMENT_3D('',#7399,#5935,#5936);
#5249=AXIS2_PLACEMENT_3D('',#7405,#5940,#5941);
#5250=AXIS2_PLACEMENT_3D('',#7411,#5945,#5946);
#5251=AXIS2_PLACEMENT_3D('',#7413,#5947,#5948);
#5252=AXIS2_PLACEMENT_3D('',#7416,#5950,#5951);
#5253=AXIS2_PLACEMENT_3D('',#7417,#5952,#5953);
#5254=AXIS2_PLACEMENT_3D('',#7423,#5957,#5958);
#5255=AXIS2_PLACEMENT_3D('',#7429,#5962,#5963);
#5256=AXIS2_PLACEMENT_3D('',#7432,#5966,#5967);
#5257=AXIS2_PLACEMENT_3D('',#7438,#5971,#5972);
#5258=AXIS2_PLACEMENT_3D('',#7441,#5975,#5976);
#5259=AXIS2_PLACEMENT_3D('',#7447,#5980,#5981);
#5260=AXIS2_PLACEMENT_3D('',#7450,#5984,#5985);
#5261=AXIS2_PLACEMENT_3D('',#7453,#5988,#5989);
#5262=AXIS2_PLACEMENT_3D('',#7454,#5990,#5991);
#5263=AXIS2_PLACEMENT_3D('',#7455,#5992,#5993);
#5264=AXIS2_PLACEMENT_3D('',#7456,#5994,#5995);
#5265=AXIS2_PLACEMENT_3D('',#7465,#6000,#6001);
#5266=AXIS2_PLACEMENT_3D('',#7471,#6005,#6006);
#5267=AXIS2_PLACEMENT_3D('',#7478,#6010,#6011);
#5268=AXIS2_PLACEMENT_3D('',#7479,#6012,#6013);
#5269=AXIS2_PLACEMENT_3D('',#7493,#6021,#6022);
#5270=AXIS2_PLACEMENT_3D('',#7497,#6025,#6026);
#5271=AXIS2_PLACEMENT_3D('',#7501,#6029,#6030);
#5272=AXIS2_PLACEMENT_3D('',#7511,#6036,#6037);
#5273=AXIS2_PLACEMENT_3D('',#7513,#6039,#6040);
#5274=AXIS2_PLACEMENT_3D('',#7517,#6042,#6043);
#5275=AXIS2_PLACEMENT_3D('',#7519,#6045,#6046);
#5276=AXIS2_PLACEMENT_3D('',#7521,#6047,#6048);
#5277=AXIS2_PLACEMENT_3D('',#7524,#6050,#6051);
#5278=AXIS2_PLACEMENT_3D('',#7526,#6052,#6053);
#5279=AXIS2_PLACEMENT_3D('',#7527,#6054,#6055);
#5280=AXIS2_PLACEMENT_3D('',#7528,#6056,#6057);
#5281=AXIS2_PLACEMENT_3D('',#7530,#6059,#6060);
#5282=AXIS2_PLACEMENT_3D('',#7532,#6062,#6063);
#5283=AXIS2_PLACEMENT_3D('',#7534,#6065,#6066);
#5284=AXIS2_PLACEMENT_3D('',#7535,#6067,#6068);
#5285=AXIS2_PLACEMENT_3D('',#7536,#6069,#6070);
#5286=AXIS2_PLACEMENT_3D('',#7545,#6075,#6076);
#5287=AXIS2_PLACEMENT_3D('',#7551,#6080,#6081);
#5288=AXIS2_PLACEMENT_3D('',#7557,#6085,#6086);
#5289=AXIS2_PLACEMENT_3D('',#7563,#6090,#6091);
#5290=AXIS2_PLACEMENT_3D('',#7569,#6095,#6096);
#5291=AXIS2_PLACEMENT_3D('',#7572,#6099,#6100);
#5292=AXIS2_PLACEMENT_3D('',#7573,#6101,#6102);
#5293=AXIS2_PLACEMENT_3D('',#7574,#6103,#6104);
#5294=AXIS2_PLACEMENT_3D('',#7576,#6105,#6106);
#5295=AXIS2_PLACEMENT_3D('',#7577,#6107,#6108);
#5296=AXIS2_PLACEMENT_3D('',#7579,#6109,#6110);
#5297=AXIS2_PLACEMENT_3D('',#7580,#6111,#6112);
#5298=AXIS2_PLACEMENT_3D('',#7582,#6113,#6114);
#5299=AXIS2_PLACEMENT_3D('',#7584,#6116,#6117);
#5300=AXIS2_PLACEMENT_3D('',#7586,#6118,#6119);
#5301=AXIS2_PLACEMENT_3D('',#7588,#6121,#6122);
#5302=AXIS2_PLACEMENT_3D('',#7590,#6123,#6124);
#5303=AXIS2_PLACEMENT_3D('',#7592,#6126,#6127);
#5304=AXIS2_PLACEMENT_3D('',#7594,#6128,#6129);
#5305=AXIS2_PLACEMENT_3D('',#7595,#6130,#6131);
#5306=AXIS2_PLACEMENT_3D('',#7597,#6132,#6133);
#5307=AXIS2_PLACEMENT_3D('',#7599,#6135,#6136);
#5308=AXIS2_PLACEMENT_3D('',#7601,#6138,#6139);
#5309=AXIS2_PLACEMENT_3D('',#7602,#6140,#6141);
#5310=AXIS2_PLACEMENT_3D('',#7604,#6142,#6143);
#5311=AXIS2_PLACEMENT_3D('',#7607,#6145,#6146);
#5312=AXIS2_PLACEMENT_3D('',#7608,#6147,#6148);
#5313=AXIS2_PLACEMENT_3D('',#7610,#6149,#6150);
#5314=AXIS2_PLACEMENT_3D('',#7611,#6151,#6152);
#5315=AXIS2_PLACEMENT_3D('',#7613,#6153,#6154);
#5316=AXIS2_PLACEMENT_3D('',#7616,#6156,#6157);
#5317=AXIS2_PLACEMENT_3D('',#7617,#6158,#6159);
#5318=AXIS2_PLACEMENT_3D('',#7619,#6160,#6161);
#5319=AXIS2_PLACEMENT_3D('',#7620,#6162,#6163);
#5320=AXIS2_PLACEMENT_3D('',#7622,#6164,#6165);
#5321=AXIS2_PLACEMENT_3D('',#7625,#6167,#6168);
#5322=AXIS2_PLACEMENT_3D('',#7626,#6169,#6170);
#5323=AXIS2_PLACEMENT_3D('',#7628,#6171,#6172);
#5324=AXIS2_PLACEMENT_3D('',#7629,#6173,#6174);
#5325=AXIS2_PLACEMENT_3D('',#7631,#6175,#6176);
#5326=AXIS2_PLACEMENT_3D('',#7634,#6178,#6179);
#5327=AXIS2_PLACEMENT_3D('',#7635,#6180,#6181);
#5328=AXIS2_PLACEMENT_3D('',#7637,#6182,#6183);
#5329=AXIS2_PLACEMENT_3D('',#7638,#6184,#6185);
#5330=AXIS2_PLACEMENT_3D('',#7640,#6186,#6187);
#5331=AXIS2_PLACEMENT_3D('',#7642,#6189,#6190);
#5332=AXIS2_PLACEMENT_3D('',#7644,#6191,#6192);
#5333=AXIS2_PLACEMENT_3D('',#7646,#6194,#6195);
#5334=AXIS2_PLACEMENT_3D('',#7648,#6196,#6197);
#5335=AXIS2_PLACEMENT_3D('',#7650,#6199,#6200);
#5336=AXIS2_PLACEMENT_3D('',#7652,#6201,#6202);
#5337=AXIS2_PLACEMENT_3D('',#7654,#6204,#6205);
#5338=AXIS2_PLACEMENT_3D('',#7663,#6210,#6211);
#5339=AXIS2_PLACEMENT_3D('',#7669,#6215,#6216);
#5340=AXIS2_PLACEMENT_3D('',#7675,#6220,#6221);
#5341=AXIS2_PLACEMENT_3D('',#7681,#6225,#6226);
#5342=AXIS2_PLACEMENT_3D('',#7687,#6230,#6231);
#5343=AXIS2_PLACEMENT_3D('',#7693,#6235,#6236);
#5344=AXIS2_PLACEMENT_3D('',#7699,#6240,#6241);
#5345=AXIS2_PLACEMENT_3D('',#7705,#6245,#6246);
#5346=AXIS2_PLACEMENT_3D('',#7711,#6250,#6251);
#5347=AXIS2_PLACEMENT_3D('',#7717,#6255,#6256);
#5348=AXIS2_PLACEMENT_3D('',#7723,#6260,#6261);
#5349=AXIS2_PLACEMENT_3D('',#7726,#6264,#6265);
#5350=AXIS2_PLACEMENT_3D('',#7727,#6266,#6267);
#5351=AXIS2_PLACEMENT_3D('',#7728,#6268,#6269);
#5352=AXIS2_PLACEMENT_3D('',#7729,#6270,#6271);
#5353=AXIS2_PLACEMENT_3D('',#7731,#6272,#6273);
#5354=AXIS2_PLACEMENT_3D('',#7732,#6274,#6275);
#5355=AXIS2_PLACEMENT_3D('',#7734,#6276,#6277);
#5356=AXIS2_PLACEMENT_3D('',#7736,#6279,#6280);
#5357=AXIS2_PLACEMENT_3D('',#7738,#6281,#6282);
#5358=AXIS2_PLACEMENT_3D('',#7740,#6284,#6285);
#5359=AXIS2_PLACEMENT_3D('',#7742,#6286,#6287);
#5360=AXIS2_PLACEMENT_3D('',#7744,#6289,#6290);
#5361=AXIS2_PLACEMENT_3D('',#7746,#6291,#6292);
#5362=AXIS2_PLACEMENT_3D('',#7747,#6293,#6294);
#5363=AXIS2_PLACEMENT_3D('',#7749,#6295,#6296);
#5364=AXIS2_PLACEMENT_3D('',#7751,#6298,#6299);
#5365=AXIS2_PLACEMENT_3D('',#7753,#6300,#6301);
#5366=AXIS2_PLACEMENT_3D('',#7755,#6303,#6304);
#5367=AXIS2_PLACEMENT_3D('',#7757,#6305,#6306);
#5368=AXIS2_PLACEMENT_3D('',#7759,#6308,#6309);
#5369=AXIS2_PLACEMENT_3D('',#7760,#6310,#6311);
#5370=AXIS2_PLACEMENT_3D('',#7769,#6316,#6317);
#5371=AXIS2_PLACEMENT_3D('',#7775,#6321,#6322);
#5372=AXIS2_PLACEMENT_3D('',#7781,#6326,#6327);
#5373=AXIS2_PLACEMENT_3D('',#7787,#6331,#6332);
#5374=AXIS2_PLACEMENT_3D('',#7793,#6336,#6337);
#5375=AXIS2_PLACEMENT_3D('',#7796,#6340,#6341);
#5376=AXIS2_PLACEMENT_3D('',#7797,#6342,#6343);
#5377=AXIS2_PLACEMENT_3D('',#7798,#6344,#6345);
#5378=AXIS2_PLACEMENT_3D('',#7799,#6346,#6347);
#5379=AXIS2_PLACEMENT_3D('',#7801,#6348,#6349);
#5380=AXIS2_PLACEMENT_3D('',#7804,#6351,#6352);
#5381=AXIS2_PLACEMENT_3D('',#7805,#6353,#6354);
#5382=AXIS2_PLACEMENT_3D('',#7807,#6355,#6356);
#5383=AXIS2_PLACEMENT_3D('',#7808,#6357,#6358);
#5384=AXIS2_PLACEMENT_3D('',#7810,#6359,#6360);
#5385=AXIS2_PLACEMENT_3D('',#7813,#6362,#6363);
#5386=AXIS2_PLACEMENT_3D('',#7814,#6364,#6365);
#5387=AXIS2_PLACEMENT_3D('',#7816,#6366,#6367);
#5388=AXIS2_PLACEMENT_3D('',#7817,#6368,#6369);
#5389=AXIS2_PLACEMENT_3D('',#7819,#6370,#6371);
#5390=AXIS2_PLACEMENT_3D('',#7821,#6373,#6374);
#5391=AXIS2_PLACEMENT_3D('',#7823,#6375,#6376);
#5392=AXIS2_PLACEMENT_3D('',#7825,#6378,#6379);
#5393=AXIS2_PLACEMENT_3D('',#7834,#6384,#6385);
#5394=AXIS2_PLACEMENT_3D('',#7840,#6389,#6390);
#5395=AXIS2_PLACEMENT_3D('',#7846,#6394,#6395);
#5396=AXIS2_PLACEMENT_3D('',#7849,#6398,#6399);
#5397=AXIS2_PLACEMENT_3D('',#7850,#6400,#6401);
#5398=AXIS2_PLACEMENT_3D('',#7851,#6402,#6403);
#5399=AXIS2_PLACEMENT_3D('',#7852,#6404,#6405);
#5400=AXIS2_PLACEMENT_3D('',#7861,#6410,#6411);
#5401=AXIS2_PLACEMENT_3D('',#7867,#6415,#6416);
#5402=AXIS2_PLACEMENT_3D('',#7873,#6420,#6421);
#5403=AXIS2_PLACEMENT_3D('',#7876,#6424,#6425);
#5404=AXIS2_PLACEMENT_3D('',#7877,#6426,#6427);
#5405=AXIS2_PLACEMENT_3D('',#7878,#6428,#6429);
#5406=AXIS2_PLACEMENT_3D('',#7879,#6430,#6431);
#5407=AXIS2_PLACEMENT_3D('',#7888,#6436,#6437);
#5408=AXIS2_PLACEMENT_3D('',#7894,#6441,#6442);
#5409=AXIS2_PLACEMENT_3D('',#7900,#6446,#6447);
#5410=AXIS2_PLACEMENT_3D('',#7903,#6450,#6451);
#5411=AXIS2_PLACEMENT_3D('',#7904,#6452,#6453);
#5412=AXIS2_PLACEMENT_3D('',#7905,#6454,#6455);
#5413=AXIS2_PLACEMENT_3D('',#7906,#6456,#6457);
#5414=AXIS2_PLACEMENT_3D('',#7907,#6458,#6459);
#5415=AXIS2_PLACEMENT_3D('',#7908,#6460,#6461);
#5416=AXIS2_PLACEMENT_3D('',#7912,#6463,#6464);
#5417=AXIS2_PLACEMENT_3D('',#7913,#6465,#6466);
#5418=AXIS2_PLACEMENT_3D('',#7917,#6468,#6469);
#5419=AXIS2_PLACEMENT_3D('',#7920,#6471,#6472);
#5420=AXIS2_PLACEMENT_3D('',#7922,#6473,#6474);
#5421=AXIS2_PLACEMENT_3D('',#7924,#6476,#6477);
#5422=AXIS2_PLACEMENT_3D('',#7928,#6479,#6480);
#5423=AXIS2_PLACEMENT_3D('',#7929,#6481,#6482);
#5424=AXIS2_PLACEMENT_3D('',#7933,#6484,#6485);
#5425=AXIS2_PLACEMENT_3D('',#7936,#6487,#6488);
#5426=AXIS2_PLACEMENT_3D('',#7938,#6489,#6490);
#5427=AXIS2_PLACEMENT_3D('',#7940,#6492,#6493);
#5428=AXIS2_PLACEMENT_3D('',#7944,#6495,#6496);
#5429=AXIS2_PLACEMENT_3D('',#7945,#6497,#6498);
#5430=AXIS2_PLACEMENT_3D('',#7949,#6500,#6501);
#5431=AXIS2_PLACEMENT_3D('',#7952,#6503,#6504);
#5432=AXIS2_PLACEMENT_3D('',#7954,#6505,#6506);
#5433=AXIS2_PLACEMENT_3D('',#7956,#6508,#6509);
#5434=AXIS2_PLACEMENT_3D('',#7960,#6511,#6512);
#5435=AXIS2_PLACEMENT_3D('',#7961,#6513,#6514);
#5436=AXIS2_PLACEMENT_3D('',#7965,#6516,#6517);
#5437=AXIS2_PLACEMENT_3D('',#7968,#6519,#6520);
#5438=AXIS2_PLACEMENT_3D('',#7970,#6521,#6522);
#5439=AXIS2_PLACEMENT_3D('',#7972,#6524,#6525);
#5440=AXIS2_PLACEMENT_3D('',#7983,#6532,#6533);
#5441=AXIS2_PLACEMENT_3D('',#7994,#6540,#6541);
#5442=AXIS2_PLACEMENT_3D('',#8013,#6552,#6553);
#5443=AXIS2_PLACEMENT_3D('',#8017,#6556,#6557);
#5444=AXIS2_PLACEMENT_3D('',#8021,#6560,#6561);
#5445=AXIS2_PLACEMENT_3D('',#8025,#6564,#6565);
#5446=AXIS2_PLACEMENT_3D('',#8029,#6568,#6569);
#5447=AXIS2_PLACEMENT_3D('',#8031,#6571,#6572);
#5448=AXIS2_PLACEMENT_3D('',#8035,#6575,#6576);
#5449=AXIS2_PLACEMENT_3D('',#8039,#6579,#6580);
#5450=AXIS2_PLACEMENT_3D('',#8043,#6583,#6584);
#5451=AXIS2_PLACEMENT_3D('',#8047,#6587,#6588);
#5452=AXIS2_PLACEMENT_3D('',#8049,#6590,#6591);
#5453=AXIS2_PLACEMENT_3D('',#8050,#6592,#6593);
#5454=AXIS2_PLACEMENT_3D('',#8051,#6594,#6595);
#5455=AXIS2_PLACEMENT_3D('',#8060,#6600,#6601);
#5456=AXIS2_PLACEMENT_3D('',#8066,#6605,#6606);
#5457=AXIS2_PLACEMENT_3D('',#8072,#6610,#6611);
#5458=AXIS2_PLACEMENT_3D('',#8078,#6615,#6616);
#5459=AXIS2_PLACEMENT_3D('',#8084,#6620,#6621);
#5460=AXIS2_PLACEMENT_3D('',#8090,#6625,#6626);
#5461=AXIS2_PLACEMENT_3D('',#8096,#6630,#6631);
#5462=AXIS2_PLACEMENT_3D('',#8099,#6634,#6635);
#5463=AXIS2_PLACEMENT_3D('',#8100,#6636,#6637);
#5464=AXIS2_PLACEMENT_3D('',#8101,#6638,#6639);
#5465=AXIS2_PLACEMENT_3D('',#8102,#6640,#6641);
#5466=AXIS2_PLACEMENT_3D('',#8111,#6646,#6647);
#5467=AXIS2_PLACEMENT_3D('',#8117,#6651,#6652);
#5468=AXIS2_PLACEMENT_3D('',#8123,#6656,#6657);
#5469=AXIS2_PLACEMENT_3D('',#8129,#6661,#6662);
#5470=AXIS2_PLACEMENT_3D('',#8135,#6666,#6667);
#5471=AXIS2_PLACEMENT_3D('',#8141,#6671,#6672);
#5472=AXIS2_PLACEMENT_3D('',#8147,#6676,#6677);
#5473=AXIS2_PLACEMENT_3D('',#8150,#6680,#6681);
#5474=AXIS2_PLACEMENT_3D('',#8151,#6682,#6683);
#5475=AXIS2_PLACEMENT_3D('',#8152,#6684,#6685);
#5476=AXIS2_PLACEMENT_3D('',#8153,#6686,#6687);
#5477=AXIS2_PLACEMENT_3D('',#8154,#6688,#6689);
#5478=AXIS2_PLACEMENT_3D('',#8155,#6690,#6691);
#5479=AXIS2_PLACEMENT_3D('',#8156,#6692,#6693);
#5480=AXIS2_PLACEMENT_3D('',#8158,#6694,#6695);
#5481=AXIS2_PLACEMENT_3D('',#8161,#6697,#6698);
#5482=AXIS2_PLACEMENT_3D('',#8162,#6699,#6700);
#5483=AXIS2_PLACEMENT_3D('',#8164,#6701,#6702);
#5484=AXIS2_PLACEMENT_3D('',#8167,#6704,#6705);
#5485=AXIS2_PLACEMENT_3D('',#8168,#6706,#6707);
#5486=AXIS2_PLACEMENT_3D('',#8170,#6708,#6709);
#5487=AXIS2_PLACEMENT_3D('',#8173,#6711,#6712);
#5488=AXIS2_PLACEMENT_3D('',#8174,#6713,#6714);
#5489=AXIS2_PLACEMENT_3D('',#8176,#6715,#6716);
#5490=AXIS2_PLACEMENT_3D('',#8179,#6718,#6719);
#5491=AXIS2_PLACEMENT_3D('',#8180,#6720,#6721);
#5492=AXIS2_PLACEMENT_3D('',#8182,#6722,#6723);
#5493=AXIS2_PLACEMENT_3D('',#8185,#6725,#6726);
#5494=AXIS2_PLACEMENT_3D('',#8186,#6727,#6728);
#5495=AXIS2_PLACEMENT_3D('',#8188,#6729,#6730);
#5496=AXIS2_PLACEMENT_3D('',#8191,#6732,#6733);
#5497=AXIS2_PLACEMENT_3D('',#8192,#6734,#6735);
#5498=AXIS2_PLACEMENT_3D('',#8201,#6740,#6741);
#5499=AXIS2_PLACEMENT_3D('',#8207,#6745,#6746);
#5500=AXIS2_PLACEMENT_3D('',#8213,#6750,#6751);
#5501=AXIS2_PLACEMENT_3D('',#8216,#6754,#6755);
#5502=AXIS2_PLACEMENT_3D('',#8217,#6756,#6757);
#5503=AXIS2_PLACEMENT_3D('',#8218,#6758,#6759);
#5504=AXIS2_PLACEMENT_3D('',#8219,#6760,#6761);
#5505=AXIS2_PLACEMENT_3D('',#8221,#6762,#6763);
#5506=AXIS2_PLACEMENT_3D('',#8224,#6765,#6766);
#5507=AXIS2_PLACEMENT_3D('',#8225,#6767,#6768);
#5508=AXIS2_PLACEMENT_3D('',#8227,#6769,#6770);
#5509=AXIS2_PLACEMENT_3D('',#8230,#6772,#6773);
#5510=AXIS2_PLACEMENT_3D('',#8231,#6774,#6775);
#5511=AXIS2_PLACEMENT_3D('',#8232,#6776,#6777);
#5512=AXIS2_PLACEMENT_3D('',#8233,#6778,#6779);
#5513=AXIS2_PLACEMENT_3D('',#8234,#6780,#6781);
#5514=AXIS2_PLACEMENT_3D('',#8236,#6782,#6783);
#5515=AXIS2_PLACEMENT_3D('',#8239,#6785,#6786);
#5516=AXIS2_PLACEMENT_3D('',#8240,#6787,#6788);
#5517=AXIS2_PLACEMENT_3D('',#8243,#6790,#6791);
#5518=AXIS2_PLACEMENT_3D('',#8244,#6792,#6793);
#5519=AXIS2_PLACEMENT_3D('',#8246,#6794,#6795);
#5520=AXIS2_PLACEMENT_3D('',#8247,#6796,#6797);
#5521=AXIS2_PLACEMENT_3D('',#8250,#6799,#6800);
#5522=AXIS2_PLACEMENT_3D('',#8251,#6801,#6802);
#5523=AXIS2_PLACEMENT_3D('',#8252,#6803,#6804);
#5524=AXIS2_PLACEMENT_3D('',#8253,#6805,#6806);
#5525=AXIS2_PLACEMENT_3D('',#8255,#6807,#6808);
#5526=AXIS2_PLACEMENT_3D('',#8256,#6809,#6810);
#5527=AXIS2_PLACEMENT_3D('',#8258,#6811,#6812);
#5528=AXIS2_PLACEMENT_3D('',#8260,#6814,#6815);
#5529=AXIS2_PLACEMENT_3D('',#8262,#6816,#6817);
#5530=AXIS2_PLACEMENT_3D('',#8264,#6819,#6820);
#5531=AXIS2_PLACEMENT_3D('',#8266,#6821,#6822);
#5532=AXIS2_PLACEMENT_3D('',#8268,#6824,#6825);
#5533=AXIS2_PLACEMENT_3D('',#8270,#6826,#6827);
#5534=AXIS2_PLACEMENT_3D('',#8271,#6828,#6829);
#5535=AXIS2_PLACEMENT_3D('',#8273,#6830,#6831);
#5536=AXIS2_PLACEMENT_3D('',#8275,#6833,#6834);
#5537=AXIS2_PLACEMENT_3D('',#8277,#6835,#6836);
#5538=AXIS2_PLACEMENT_3D('',#8279,#6838,#6839);
#5539=AXIS2_PLACEMENT_3D('',#8281,#6840,#6841);
#5540=AXIS2_PLACEMENT_3D('',#8283,#6843,#6844);
#5541=AXIS2_PLACEMENT_3D('',#8284,#6845,#6846);
#5542=AXIS2_PLACEMENT_3D('',#8293,#6851,#6852);
#5543=AXIS2_PLACEMENT_3D('',#8299,#6856,#6857);
#5544=AXIS2_PLACEMENT_3D('',#8305,#6861,#6862);
#5545=AXIS2_PLACEMENT_3D('',#8311,#6866,#6867);
#5546=AXIS2_PLACEMENT_3D('',#8317,#6871,#6872);
#5547=AXIS2_PLACEMENT_3D('',#8320,#6875,#6876);
#5548=AXIS2_PLACEMENT_3D('',#8321,#6877,#6878);
#5549=AXIS2_PLACEMENT_3D('',#8322,#6879,#6880);
#5550=AXIS2_PLACEMENT_3D('',#8323,#6881,#6882);
#5551=AXIS2_PLACEMENT_3D('',#8324,#6883,#6884);
#5552=AXIS2_PLACEMENT_3D('',#8325,#6885,#6886);
#5553=AXIS2_PLACEMENT_3D('',#8326,#6887,#6888);
#5554=AXIS2_PLACEMENT_3D('',#8327,#6889,#6890);
#5555=AXIS2_PLACEMENT_3D('',#8328,#6891,#6892);
#5556=AXIS2_PLACEMENT_3D('',#8329,#6893,#6894);
#5557=AXIS2_PLACEMENT_3D('',#8330,#6895,#6896);
#5558=AXIS2_PLACEMENT_3D('',#8331,#6897,#6898);
#5559=AXIS2_PLACEMENT_3D('',#8332,#6899,#6900);
#5560=AXIS2_PLACEMENT_3D('',#8333,#6901,#6902);
#5561=AXIS2_PLACEMENT_3D('',#8334,#6903,#6904);
#5562=AXIS2_PLACEMENT_3D('',#8335,#6905,#6906);
#5563=AXIS2_PLACEMENT_3D('',#8336,#6907,#6908);
#5564=AXIS2_PLACEMENT_3D('',#8337,#6909,#6910);
#5565=AXIS2_PLACEMENT_3D('',#8338,#6911,#6912);
#5566=AXIS2_PLACEMENT_3D('',#8339,#6913,#6914);
#5567=AXIS2_PLACEMENT_3D('',#8340,#6915,#6916);
#5568=AXIS2_PLACEMENT_3D('',#8341,#6917,#6918);
#5569=AXIS2_PLACEMENT_3D('',#8342,#6919,#6920);
#5570=AXIS2_PLACEMENT_3D('',#8343,#6921,#6922);
#5571=AXIS2_PLACEMENT_3D('',#8344,#6923,#6924);
#5572=AXIS2_PLACEMENT_3D('',#8345,#6925,#6926);
#5573=AXIS2_PLACEMENT_3D('',#8346,#6927,#6928);
#5574=AXIS2_PLACEMENT_3D('',#8347,#6929,#6930);
#5575=AXIS2_PLACEMENT_3D('',#8348,#6931,#6932);
#5576=AXIS2_PLACEMENT_3D('',#8349,#6933,#6934);
#5577=AXIS2_PLACEMENT_3D('',#8350,#6935,#6936);
#5578=AXIS2_PLACEMENT_3D('',#8351,#6937,#6938);
#5579=AXIS2_PLACEMENT_3D('',#8352,#6939,#6940);
#5580=AXIS2_PLACEMENT_3D('',#8353,#6941,#6942);
#5581=AXIS2_PLACEMENT_3D('',#8354,#6943,#6944);
#5582=AXIS2_PLACEMENT_3D('',#8355,#6945,#6946);
#5583=AXIS2_PLACEMENT_3D('',#8357,#6947,#6948);
#5584=AXIS2_PLACEMENT_3D('',#8360,#6950,#6951);
#5585=AXIS2_PLACEMENT_3D('',#8361,#6952,#6953);
#5586=AXIS2_PLACEMENT_3D('',#8363,#6954,#6955);
#5587=AXIS2_PLACEMENT_3D('',#8366,#6957,#6958);
#5588=AXIS2_PLACEMENT_3D('',#8367,#6959,#6960);
#5589=AXIS2_PLACEMENT_3D('',#8368,#6961,#6962);
#5590=AXIS2_PLACEMENT_3D('',#8369,#6963,#6964);
#5591=AXIS2_PLACEMENT_3D('',#8370,#6965,#6966);
#5592=AXIS2_PLACEMENT_3D('',#8372,#6967,#6968);
#5593=AXIS2_PLACEMENT_3D('',#8373,#6969,#6970);
#5594=AXIS2_PLACEMENT_3D('',#8375,#6971,#6972);
#5595=AXIS2_PLACEMENT_3D('',#8377,#6974,#6975);
#5596=AXIS2_PLACEMENT_3D('',#8379,#6976,#6977);
#5597=AXIS2_PLACEMENT_3D('',#8381,#6979,#6980);
#5598=AXIS2_PLACEMENT_3D('',#8383,#6981,#6982);
#5599=AXIS2_PLACEMENT_3D('',#8385,#6984,#6985);
#5600=AXIS2_PLACEMENT_3D('',#8387,#6986,#6987);
#5601=AXIS2_PLACEMENT_3D('',#8388,#6988,#6989);
#5602=AXIS2_PLACEMENT_3D('',#8390,#6990,#6991);
#5603=AXIS2_PLACEMENT_3D('',#8392,#6993,#6994);
#5604=AXIS2_PLACEMENT_3D('',#8394,#6995,#6996);
#5605=AXIS2_PLACEMENT_3D('',#8396,#6998,#6999);
#5606=AXIS2_PLACEMENT_3D('',#8398,#7000,#7001);
#5607=AXIS2_PLACEMENT_3D('',#8400,#7003,#7004);
#5608=AXIS2_PLACEMENT_3D('',#8401,#7005,#7006);
#5609=AXIS2_PLACEMENT_3D('',#8410,#7011,#7012);
#5610=AXIS2_PLACEMENT_3D('',#8416,#7016,#7017);
#5611=AXIS2_PLACEMENT_3D('',#8422,#7021,#7022);
#5612=AXIS2_PLACEMENT_3D('',#8428,#7026,#7027);
#5613=AXIS2_PLACEMENT_3D('',#8434,#7031,#7032);
#5614=AXIS2_PLACEMENT_3D('',#8437,#7035,#7036);
#5615=AXIS2_PLACEMENT_3D('',#8438,#7037,#7038);
#5616=AXIS2_PLACEMENT_3D('',#8439,#7039,#7040);
#5617=AXIS2_PLACEMENT_3D('',#8440,#7041,#7042);
#5618=AXIS2_PLACEMENT_3D('',#8441,#7043,#7044);
#5619=AXIS2_PLACEMENT_3D('',#8442,#7045,#7046);
#5620=AXIS2_PLACEMENT_3D('',#8443,#7047,#7048);
#5621=AXIS2_PLACEMENT_3D('',#8444,#7049,#7050);
#5622=AXIS2_PLACEMENT_3D('',#8445,#7051,#7052);
#5623=AXIS2_PLACEMENT_3D('',#8446,#7053,#7054);
#5624=AXIS2_PLACEMENT_3D('',#8447,#7055,#7056);
#5625=AXIS2_PLACEMENT_3D('',#8448,#7057,#7058);
#5626=AXIS2_PLACEMENT_3D('',#8449,#7059,#7060);
#5627=AXIS2_PLACEMENT_3D('',#8450,#7061,#7062);
#5628=AXIS2_PLACEMENT_3D('',#8451,#7063,#7064);
#5629=AXIS2_PLACEMENT_3D('',#8452,#7065,#7066);
#5630=AXIS2_PLACEMENT_3D('',#8453,#7067,#7068);
#5631=DIRECTION('axis',(0.,0.,1.));
#5632=DIRECTION('refdir',(1.,0.,0.));
#5633=DIRECTION('axis',(0.,0.,1.));
#5634=DIRECTION('refdir',(1.,0.,0.));
#5635=DIRECTION('axis',(0.,0.,1.));
#5636=DIRECTION('refdir',(1.,0.,0.));
#5637=DIRECTION('center_axis',(0.,0.,1.));
#5638=DIRECTION('ref_axis',(1.,0.,0.));
#5639=DIRECTION('center_axis',(0.,0.,1.));
#5640=DIRECTION('ref_axis',(1.,0.,0.));
#5641=DIRECTION('',(0.,0.,1.));
#5642=DIRECTION('center_axis',(0.,0.,-1.));
#5643=DIRECTION('ref_axis',(1.,0.,0.));
#5644=DIRECTION('center_axis',(0.,0.,1.));
#5645=DIRECTION('ref_axis',(1.,0.,0.));
#5646=DIRECTION('center_axis',(0.,0.,1.));
#5647=DIRECTION('ref_axis',(1.,0.,0.));
#5648=DIRECTION('',(0.,0.,1.));
#5649=DIRECTION('center_axis',(0.,0.,-1.));
#5650=DIRECTION('ref_axis',(1.,0.,0.));
#5651=DIRECTION('center_axis',(0.,0.,1.));
#5652=DIRECTION('ref_axis',(1.,0.,0.));
#5653=DIRECTION('center_axis',(0.,0.,1.));
#5654=DIRECTION('ref_axis',(1.,0.,0.));
#5655=DIRECTION('',(0.,0.,1.));
#5656=DIRECTION('center_axis',(0.,0.,-1.));
#5657=DIRECTION('ref_axis',(1.,0.,0.));
#5658=DIRECTION('center_axis',(0.,0.,1.));
#5659=DIRECTION('ref_axis',(1.,0.,0.));
#5660=DIRECTION('center_axis',(0.,0.,1.));
#5661=DIRECTION('ref_axis',(1.,0.,0.));
#5662=DIRECTION('',(0.,0.,1.));
#5663=DIRECTION('center_axis',(0.,0.,-1.));
#5664=DIRECTION('ref_axis',(1.,0.,0.));
#5665=DIRECTION('center_axis',(0.,0.,1.));
#5666=DIRECTION('ref_axis',(1.,0.,0.));
#5667=DIRECTION('center_axis',(0.,0.,1.));
#5668=DIRECTION('ref_axis',(1.,0.,0.));
#5669=DIRECTION('',(0.,0.,1.));
#5670=DIRECTION('center_axis',(0.,0.,-1.));
#5671=DIRECTION('ref_axis',(1.,0.,0.));
#5672=DIRECTION('center_axis',(0.,0.,1.));
#5673=DIRECTION('ref_axis',(1.,0.,0.));
#5674=DIRECTION('center_axis',(0.,0.,1.));
#5675=DIRECTION('ref_axis',(1.,0.,0.));
#5676=DIRECTION('',(0.,0.,1.));
#5677=DIRECTION('center_axis',(0.,0.,-1.));
#5678=DIRECTION('ref_axis',(1.,0.,0.));
#5679=DIRECTION('center_axis',(0.,0.,1.));
#5680=DIRECTION('ref_axis',(1.,0.,0.));
#5681=DIRECTION('center_axis',(0.,0.,1.));
#5682=DIRECTION('ref_axis',(1.,0.,0.));
#5683=DIRECTION('',(0.,0.,1.));
#5684=DIRECTION('center_axis',(0.,0.,-1.));
#5685=DIRECTION('ref_axis',(1.,0.,0.));
#5686=DIRECTION('center_axis',(0.,0.,1.));
#5687=DIRECTION('ref_axis',(1.,0.,0.));
#5688=DIRECTION('center_axis',(0.,0.,1.));
#5689=DIRECTION('ref_axis',(1.,0.,0.));
#5690=DIRECTION('',(0.,0.,1.));
#5691=DIRECTION('center_axis',(0.,0.,-1.));
#5692=DIRECTION('ref_axis',(1.,0.,0.));
#5693=DIRECTION('center_axis',(0.,0.,1.));
#5694=DIRECTION('ref_axis',(1.,0.,0.));
#5695=DIRECTION('center_axis',(0.,0.,1.));
#5696=DIRECTION('ref_axis',(1.,0.,0.));
#5697=DIRECTION('',(0.,0.,1.));
#5698=DIRECTION('center_axis',(0.,0.,-1.));
#5699=DIRECTION('ref_axis',(1.,0.,0.));
#5700=DIRECTION('center_axis',(0.,0.,1.));
#5701=DIRECTION('ref_axis',(1.,0.,0.));
#5702=DIRECTION('center_axis',(0.,0.,1.));
#5703=DIRECTION('ref_axis',(1.,0.,0.));
#5704=DIRECTION('',(0.,0.,1.));
#5705=DIRECTION('center_axis',(0.,0.,-1.));
#5706=DIRECTION('ref_axis',(1.,0.,0.));
#5707=DIRECTION('center_axis',(0.,0.,1.));
#5708=DIRECTION('ref_axis',(1.,0.,0.));
#5709=DIRECTION('center_axis',(0.,0.,1.));
#5710=DIRECTION('ref_axis',(1.,0.,0.));
#5711=DIRECTION('',(0.,0.,1.));
#5712=DIRECTION('center_axis',(0.,0.,-1.));
#5713=DIRECTION('ref_axis',(1.,0.,0.));
#5714=DIRECTION('center_axis',(0.,0.,1.));
#5715=DIRECTION('ref_axis',(1.,0.,0.));
#5716=DIRECTION('center_axis',(0.,0.,1.));
#5717=DIRECTION('ref_axis',(1.,0.,0.));
#5718=DIRECTION('',(0.,0.,1.));
#5719=DIRECTION('center_axis',(0.,0.,-1.));
#5720=DIRECTION('ref_axis',(1.,0.,0.));
#5721=DIRECTION('center_axis',(0.,0.,1.));
#5722=DIRECTION('ref_axis',(1.,0.,0.));
#5723=DIRECTION('center_axis',(0.,0.,1.));
#5724=DIRECTION('ref_axis',(1.,0.,0.));
#5725=DIRECTION('',(0.,0.,1.));
#5726=DIRECTION('center_axis',(0.,0.,-1.));
#5727=DIRECTION('ref_axis',(1.,0.,0.));
#5728=DIRECTION('center_axis',(0.,0.,1.));
#5729=DIRECTION('ref_axis',(1.,0.,0.));
#5730=DIRECTION('center_axis',(0.,0.,1.));
#5731=DIRECTION('ref_axis',(1.,0.,0.));
#5732=DIRECTION('',(0.,0.,1.));
#5733=DIRECTION('center_axis',(0.,0.,-1.));
#5734=DIRECTION('ref_axis',(1.,0.,0.));
#5735=DIRECTION('center_axis',(0.,1.,0.));
#5736=DIRECTION('ref_axis',(-1.,0.,0.));
#5737=DIRECTION('',(-1.,0.,0.));
#5738=DIRECTION('',(0.,0.,1.));
#5739=DIRECTION('',(-1.,0.,0.));
#5740=DIRECTION('',(0.,0.,1.));
#5741=DIRECTION('center_axis',(1.,0.,0.));
#5742=DIRECTION('ref_axis',(0.,1.,0.));
#5743=DIRECTION('',(0.,1.,0.));
#5744=DIRECTION('',(0.,1.,0.));
#5745=DIRECTION('',(0.,0.,1.));
#5746=DIRECTION('center_axis',(0.,-1.,0.));
#5747=DIRECTION('ref_axis',(1.,0.,0.));
#5748=DIRECTION('',(1.,0.,0.));
#5749=DIRECTION('',(1.,0.,0.));
#5750=DIRECTION('',(0.,0.,1.));
#5751=DIRECTION('center_axis',(-1.,0.,0.));
#5752=DIRECTION('ref_axis',(0.,-1.,0.));
#5753=DIRECTION('',(0.,-1.,0.));
#5754=DIRECTION('',(0.,-1.,0.));
#5755=DIRECTION('center_axis',(0.,0.,1.));
#5756=DIRECTION('ref_axis',(1.,0.,0.));
#5757=DIRECTION('center_axis',(0.,0.,1.));
#5758=DIRECTION('ref_axis',(1.,0.,0.));
#5759=DIRECTION('axis',(0.,0.,1.));
#5760=DIRECTION('refdir',(1.,0.,0.));
#5761=DIRECTION('center_axis',(0.,0.,-1.));
#5762=DIRECTION('ref_axis',(0.,1.,0.));
#5763=DIRECTION('',(0.,1.,0.));
#5764=DIRECTION('',(1.,0.,0.));
#5765=DIRECTION('',(0.,-1.,0.));
#5766=DIRECTION('',(1.,0.,0.));
#5767=DIRECTION('center_axis',(0.,1.,-8.88178419700125E-16));
#5768=DIRECTION('ref_axis',(0.,8.88178419700125E-16,1.));
#5769=DIRECTION('',(0.,8.88178419700125E-16,1.));
#5770=DIRECTION('',(1.,0.,0.));
#5771=DIRECTION('',(0.,-8.88178419700125E-16,-1.));
#5772=DIRECTION('center_axis',(0.,-7.40148683083439E-16,-1.));
#5773=DIRECTION('ref_axis',(0.,1.,-7.40148683083439E-16));
#5774=DIRECTION('',(0.,1.,-7.40148683083439E-16));
#5775=DIRECTION('',(1.,0.,0.));
#5776=DIRECTION('',(0.,-1.,7.40148683083439E-16));
#5777=DIRECTION('center_axis',(0.,-0.707106781186547,-0.707106781186548));
#5778=DIRECTION('ref_axis',(0.,0.707106781186548,-0.707106781186547));
#5779=DIRECTION('',(0.,0.707106781186548,-0.707106781186547));
#5780=DIRECTION('',(1.,0.,0.));
#5781=DIRECTION('',(0.,-0.707106781186548,0.707106781186547));
#5782=DIRECTION('center_axis',(0.,-1.,2.77555756156289E-16));
#5783=DIRECTION('ref_axis',(0.,-2.77555756156289E-16,-1.));
#5784=DIRECTION('',(0.,-2.77555756156289E-16,-1.));
#5785=DIRECTION('',(1.,0.,0.));
#5786=DIRECTION('',(0.,2.77555756156289E-16,1.));
#5787=DIRECTION('center_axis',(0.,-0.707106781186547,0.707106781186548));
#5788=DIRECTION('ref_axis',(0.,-0.707106781186548,-0.707106781186547));
#5789=DIRECTION('',(0.,-0.707106781186548,-0.707106781186547));
#5790=DIRECTION('',(1.,0.,0.));
#5791=DIRECTION('',(0.,0.707106781186548,0.707106781186547));
#5792=DIRECTION('center_axis',(0.,7.40148683083438E-16,1.));
#5793=DIRECTION('ref_axis',(0.,-1.,7.40148683083438E-16));
#5794=DIRECTION('',(0.,-1.,7.40148683083438E-16));
#5795=DIRECTION('',(1.,0.,0.));
#5796=DIRECTION('',(0.,1.,-7.40148683083438E-16));
#5797=DIRECTION('center_axis',(0.,1.,-4.44089209850063E-16));
#5798=DIRECTION('ref_axis',(0.,4.44089209850063E-16,1.));
#5799=DIRECTION('',(0.,4.44089209850063E-16,1.));
#5800=DIRECTION('',(1.,0.,0.));
#5801=DIRECTION('',(0.,-4.44089209850063E-16,-1.));
#5802=DIRECTION('center_axis',(0.,2.41352831440251E-16,1.));
#5803=DIRECTION('ref_axis',(0.,-1.,2.41352831440251E-16));
#5804=DIRECTION('',(0.,-1.,2.41352831440251E-16));
#5805=DIRECTION('',(-1.,0.,0.));
#5806=DIRECTION('',(0.,1.,-2.41352831440251E-16));
#5807=DIRECTION('center_axis',(0.,-1.,2.41352831440251E-16));
#5808=DIRECTION('ref_axis',(0.,-2.41352831440251E-16,-1.));
#5809=DIRECTION('',(0.,-2.41352831440251E-16,-1.));
#5810=DIRECTION('',(1.,0.,0.));
#5811=DIRECTION('',(0.,2.41352831440251E-16,1.));
#5812=DIRECTION('',(1.,0.,0.));
#5813=DIRECTION('center_axis',(0.,0.,-1.));
#5814=DIRECTION('ref_axis',(0.,1.,0.));
#5815=DIRECTION('',(0.,1.,0.));
#5816=DIRECTION('',(1.,0.,0.));
#5817=DIRECTION('',(0.,-1.,0.));
#5818=DIRECTION('center_axis',(0.,-1.,0.));
#5819=DIRECTION('ref_axis',(0.,0.,-1.));
#5820=DIRECTION('',(0.,0.,-1.));
#5821=DIRECTION('',(1.,0.,0.));
#5822=DIRECTION('',(0.,0.,1.));
#5823=DIRECTION('center_axis',(0.,-0.707106781186547,0.707106781186548));
#5824=DIRECTION('ref_axis',(0.,-0.707106781186548,-0.707106781186547));
#5825=DIRECTION('',(0.,-0.707106781186548,-0.707106781186547));
#5826=DIRECTION('',(1.,0.,0.));
#5827=DIRECTION('',(0.,0.707106781186548,0.707106781186547));
#5828=DIRECTION('center_axis',(0.,0.,1.));
#5829=DIRECTION('ref_axis',(0.,-1.,0.));
#5830=DIRECTION('',(0.,-1.,0.));
#5831=DIRECTION('',(1.,0.,0.));
#5832=DIRECTION('',(0.,1.,0.));
#5833=DIRECTION('center_axis',(0.,0.707106781186548,0.707106781186547));
#5834=DIRECTION('ref_axis',(0.,-0.707106781186547,0.707106781186548));
#5835=DIRECTION('',(0.,-0.707106781186547,0.707106781186548));
#5836=DIRECTION('',(1.,0.,0.));
#5837=DIRECTION('',(0.,0.707106781186547,-0.707106781186548));
#5838=DIRECTION('center_axis',(0.,1.,0.));
#5839=DIRECTION('ref_axis',(0.,0.,1.));
#5840=DIRECTION('',(0.,0.,1.));
#5841=DIRECTION('',(1.,0.,0.));
#5842=DIRECTION('',(0.,0.,-1.));
#5843=DIRECTION('center_axis',(0.,0.,-1.));
#5844=DIRECTION('ref_axis',(0.,1.,0.));
#5845=DIRECTION('',(0.,1.,0.));
#5846=DIRECTION('',(1.,0.,0.));
#5847=DIRECTION('',(0.,-1.,0.));
#5848=DIRECTION('center_axis',(0.,1.,-2.41352831440251E-16));
#5849=DIRECTION('ref_axis',(0.,2.41352831440251E-16,1.));
#5850=DIRECTION('',(0.,2.41352831440251E-16,1.));
#5851=DIRECTION('',(-1.,0.,0.));
#5852=DIRECTION('',(0.,-2.41352831440251E-16,-1.));
#5853=DIRECTION('center_axis',(0.,0.,1.));
#5854=DIRECTION('ref_axis',(0.,-1.,0.));
#5855=DIRECTION('',(0.,-1.,0.));
#5856=DIRECTION('',(1.,0.,0.));
#5857=DIRECTION('',(0.,1.,0.));
#5858=DIRECTION('',(1.,0.,0.));
#5859=DIRECTION('center_axis',(0.,-1.,0.));
#5860=DIRECTION('ref_axis',(0.,0.,-1.));
#5861=DIRECTION('',(0.,0.,-1.));
#5862=DIRECTION('',(1.,0.,0.));
#5863=DIRECTION('',(0.,0.,1.));
#5864=DIRECTION('center_axis',(0.,0.,1.));
#5865=DIRECTION('ref_axis',(0.,-1.,0.));
#5866=DIRECTION('',(0.,-1.,0.));
#5867=DIRECTION('',(1.,0.,0.));
#5868=DIRECTION('',(0.,1.,0.));
#5869=DIRECTION('center_axis',(0.,0.707106781186548,0.707106781186548));
#5870=DIRECTION('ref_axis',(0.,-0.707106781186548,0.707106781186548));
#5871=DIRECTION('',(0.,-0.707106781186548,0.707106781186548));
#5872=DIRECTION('',(1.,0.,0.));
#5873=DIRECTION('',(0.,0.707106781186548,-0.707106781186548));
#5874=DIRECTION('center_axis',(0.,1.,0.));
#5875=DIRECTION('ref_axis',(0.,0.,1.));
#5876=DIRECTION('',(0.,0.,1.));
#5877=DIRECTION('',(1.,0.,0.));
#5878=DIRECTION('',(0.,0.,-1.));
#5879=DIRECTION('center_axis',(0.,0.707106781186548,-0.707106781186547));
#5880=DIRECTION('ref_axis',(0.,0.707106781186547,0.707106781186548));
#5881=DIRECTION('',(0.,0.707106781186547,0.707106781186548));
#5882=DIRECTION('',(1.,0.,0.));
#5883=DIRECTION('',(0.,-0.707106781186547,-0.707106781186548));
#5884=DIRECTION('center_axis',(0.,-7.40148683083438E-16,-1.));
#5885=DIRECTION('ref_axis',(0.,1.,-7.40148683083438E-16));
#5886=DIRECTION('',(0.,1.,-7.40148683083438E-16));
#5887=DIRECTION('',(1.,0.,0.));
#5888=DIRECTION('',(0.,-1.,7.40148683083438E-16));
#5889=DIRECTION('center_axis',(0.,-1.,0.));
#5890=DIRECTION('ref_axis',(0.,0.,-1.));
#5891=DIRECTION('',(0.,0.,-1.));
#5892=DIRECTION('',(1.,0.,0.));
#5893=DIRECTION('',(0.,0.,1.));
#5894=DIRECTION('center_axis',(0.,0.,-1.));
#5895=DIRECTION('ref_axis',(0.,1.,0.));
#5896=DIRECTION('',(0.,1.,0.));
#5897=DIRECTION('',(-1.,0.,0.));
#5898=DIRECTION('',(0.,-1.,0.));
#5899=DIRECTION('center_axis',(0.,1.,0.));
#5900=DIRECTION('ref_axis',(0.,0.,1.));
#5901=DIRECTION('',(0.,0.,1.));
#5902=DIRECTION('',(1.,0.,0.));
#5903=DIRECTION('',(0.,0.,-1.));
#5904=DIRECTION('',(1.,0.,0.));
#5905=DIRECTION('center_axis',(0.,0.,1.));
#5906=DIRECTION('ref_axis',(0.,-1.,0.));
#5907=DIRECTION('',(0.,-1.,0.));
#5908=DIRECTION('',(1.,0.,0.));
#5909=DIRECTION('',(0.,1.,0.));
#5910=DIRECTION('center_axis',(0.,1.,0.));
#5911=DIRECTION('ref_axis',(0.,0.,1.));
#5912=DIRECTION('',(0.,0.,1.));
#5913=DIRECTION('',(1.,0.,0.));
#5914=DIRECTION('',(0.,0.,-1.));
#5915=DIRECTION('center_axis',(0.,0.707106781186547,-0.707106781186548));
#5916=DIRECTION('ref_axis',(0.,0.707106781186548,0.707106781186547));
#5917=DIRECTION('',(0.,0.707106781186548,0.707106781186547));
#5918=DIRECTION('',(1.,0.,0.));
#5919=DIRECTION('',(0.,-0.707106781186548,-0.707106781186547));
#5920=DIRECTION('center_axis',(0.,0.,-1.));
#5921=DIRECTION('ref_axis',(0.,1.,0.));
#5922=DIRECTION('',(0.,1.,0.));
#5923=DIRECTION('',(1.,0.,0.));
#5924=DIRECTION('',(0.,-1.,0.));
#5925=DIRECTION('center_axis',(0.,-0.707106781186547,-0.707106781186548));
#5926=DIRECTION('ref_axis',(0.,0.707106781186548,-0.707106781186547));
#5927=DIRECTION('',(0.,0.707106781186548,-0.707106781186547));
#5928=DIRECTION('',(1.,0.,0.));
#5929=DIRECTION('',(0.,-0.707106781186548,0.707106781186547));
#5930=DIRECTION('center_axis',(0.,-1.,0.));
#5931=DIRECTION('ref_axis',(0.,0.,-1.));
#5932=DIRECTION('',(0.,0.,-1.));
#5933=DIRECTION('',(1.,0.,0.));
#5934=DIRECTION('',(0.,0.,1.));
#5935=DIRECTION('center_axis',(0.,0.,1.));
#5936=DIRECTION('ref_axis',(0.,-1.,0.));
#5937=DIRECTION('',(0.,-1.,0.));
#5938=DIRECTION('',(1.,0.,0.));
#5939=DIRECTION('',(0.,1.,0.));
#5940=DIRECTION('center_axis',(0.,-1.,0.));
#5941=DIRECTION('ref_axis',(0.,0.,-1.));
#5942=DIRECTION('',(0.,0.,-1.));
#5943=DIRECTION('',(-1.,0.,0.));
#5944=DIRECTION('',(0.,0.,1.));
#5945=DIRECTION('center_axis',(1.,0.,0.));
#5946=DIRECTION('ref_axis',(0.,0.,-1.));
#5947=DIRECTION('center_axis',(1.,0.,0.));
#5948=DIRECTION('ref_axis',(0.,0.,-1.));
#5949=DIRECTION('',(1.,0.,0.));
#5950=DIRECTION('center_axis',(-1.,0.,0.));
#5951=DIRECTION('ref_axis',(0.,0.,-1.));
#5952=DIRECTION('center_axis',(0.,1.,0.));
#5953=DIRECTION('ref_axis',(0.,0.,1.));
#5954=DIRECTION('',(0.,0.,1.));
#5955=DIRECTION('',(1.,0.,0.));
#5956=DIRECTION('',(0.,0.,1.));
#5957=DIRECTION('center_axis',(0.,1.,0.));
#5958=DIRECTION('ref_axis',(0.,0.,1.));
#5959=DIRECTION('',(0.,0.,1.));
#5960=DIRECTION('',(1.,0.,0.));
#5961=DIRECTION('',(0.,0.,1.));
#5962=DIRECTION('center_axis',(0.,0.,-1.));
#5963=DIRECTION('ref_axis',(0.,1.,0.));
#5964=DIRECTION('',(0.,1.,0.));
#5965=DIRECTION('',(0.,1.,0.));
#5966=DIRECTION('center_axis',(0.,0.,-1.));
#5967=DIRECTION('ref_axis',(0.,1.,0.));
#5968=DIRECTION('',(0.,1.,0.));
#5969=DIRECTION('',(1.,0.,0.));
#5970=DIRECTION('',(0.,1.,0.));
#5971=DIRECTION('center_axis',(0.,-1.,0.));
#5972=DIRECTION('ref_axis',(0.,0.,-1.));
#5973=DIRECTION('',(0.,0.,-1.));
#5974=DIRECTION('',(0.,0.,-1.));
#5975=DIRECTION('center_axis',(0.,-1.,0.));
#5976=DIRECTION('ref_axis',(0.,0.,-1.));
#5977=DIRECTION('',(0.,0.,-1.));
#5978=DIRECTION('',(1.,0.,0.));
#5979=DIRECTION('',(0.,0.,-1.));
#5980=DIRECTION('center_axis',(0.,0.,1.));
#5981=DIRECTION('ref_axis',(0.,-1.,0.));
#5982=DIRECTION('',(0.,-1.,0.));
#5983=DIRECTION('',(0.,-1.,0.));
#5984=DIRECTION('center_axis',(0.,0.,1.));
#5985=DIRECTION('ref_axis',(0.,-1.,0.));
#5986=DIRECTION('',(0.,-1.,0.));
#5987=DIRECTION('',(0.,-1.,0.));
#5988=DIRECTION('center_axis',(1.,0.,0.));
#5989=DIRECTION('ref_axis',(0.,0.,-1.));
#5990=DIRECTION('center_axis',(1.,0.,0.));
#5991=DIRECTION('ref_axis',(0.,0.,-1.));
#5992=DIRECTION('axis',(0.,0.,1.));
#5993=DIRECTION('refdir',(1.,0.,0.));
#5994=DIRECTION('center_axis',(0.,0.,1.));
#5995=DIRECTION('ref_axis',(1.,0.,0.));
#5996=DIRECTION('',(1.,0.,0.));
#5997=DIRECTION('',(0.,-1.,0.));
#5998=DIRECTION('',(-1.,0.,0.));
#5999=DIRECTION('',(0.,1.,0.));
#6000=DIRECTION('center_axis',(0.,1.,0.));
#6001=DIRECTION('ref_axis',(-1.,0.,0.));
#6002=DIRECTION('',(0.,0.,1.));
#6003=DIRECTION('',(-1.,0.,0.));
#6004=DIRECTION('',(0.,0.,1.));
#6005=DIRECTION('center_axis',(0.,0.,1.));
#6006=DIRECTION('ref_axis',(1.,0.,0.));
#6007=DIRECTION('',(0.,-1.,0.));
#6008=DIRECTION('',(1.,0.,0.));
#6009=DIRECTION('',(0.,1.,0.));
#6010=DIRECTION('center_axis',(0.,0.,-1.));
#6011=DIRECTION('ref_axis',(1.,0.,0.));
#6012=DIRECTION('center_axis',(-1.,0.,0.));
#6013=DIRECTION('ref_axis',(0.,-1.,0.));
#6014=DIRECTION('',(0.,0.,1.));
#6015=DIRECTION('',(0.,0.707106781186548,0.707106781186548));
#6016=DIRECTION('',(0.,-1.,0.));
#6017=DIRECTION('',(0.,0.707106781186548,-0.707106781186548));
#6018=DIRECTION('',(0.,0.,1.));
#6019=DIRECTION('',(0.,-1.,0.));
#6020=DIRECTION('',(0.,0.,1.));
#6021=DIRECTION('center_axis',(0.,-1.,0.));
#6022=DIRECTION('ref_axis',(1.,0.,0.));
#6023=DIRECTION('',(1.,0.,0.));
#6024=DIRECTION('',(0.,0.,1.));
#6025=DIRECTION('center_axis',(0.,0.,1.));
#6026=DIRECTION('ref_axis',(1.,0.,0.));
#6027=DIRECTION('',(-1.,0.,0.));
#6028=DIRECTION('',(0.,1.,0.));
#6029=DIRECTION('center_axis',(1.,0.,0.));
#6030=DIRECTION('ref_axis',(0.,1.,0.));
#6031=DIRECTION('',(0.,0.,1.));
#6032=DIRECTION('',(0.,-0.707106781186548,0.707106781186548));
#6033=DIRECTION('',(0.,1.,0.));
#6034=DIRECTION('',(0.,-0.707106781186548,-0.707106781186548));
#6035=DIRECTION('',(0.,0.,1.));
#6036=DIRECTION('center_axis',(0.,-1.,0.));
#6037=DIRECTION('ref_axis',(1.,0.,0.));
#6038=DIRECTION('',(-1.,0.,0.));
#6039=DIRECTION('center_axis',(0.,-0.707106781186548,-0.707106781186548));
#6040=DIRECTION('ref_axis',(-1.,0.,0.));
#6041=DIRECTION('',(1.,0.,0.));
#6042=DIRECTION('center_axis',(0.,0.707106781186548,0.707106781186548));
#6043=DIRECTION('ref_axis',(0.,0.707106781186547,-0.707106781186547));
#6044=DIRECTION('',(1.,0.,0.));
#6045=DIRECTION('center_axis',(0.,0.,1.));
#6046=DIRECTION('ref_axis',(1.,0.,0.));
#6047=DIRECTION('center_axis',(0.,0.,-1.));
#6048=DIRECTION('ref_axis',(1.,0.,0.));
#6049=DIRECTION('',(0.,0.,1.));
#6050=DIRECTION('center_axis',(0.,0.,-1.));
#6051=DIRECTION('ref_axis',(1.,0.,0.));
#6052=DIRECTION('center_axis',(0.,-0.707106781186548,0.707106781186548));
#6053=DIRECTION('ref_axis',(0.,0.707106781186547,0.707106781186547));
#6054=DIRECTION('center_axis',(0.,0.,-1.));
#6055=DIRECTION('ref_axis',(1.,0.,0.));
#6056=DIRECTION('center_axis',(0.,0.,1.));
#6057=DIRECTION('ref_axis',(1.,0.,0.));
#6058=DIRECTION('',(-1.,0.,0.));
#6059=DIRECTION('center_axis',(0.,0.,1.));
#6060=DIRECTION('ref_axis',(1.,0.,0.));
#6061=DIRECTION('',(-1.,0.,0.));
#6062=DIRECTION('center_axis',(0.,0.707106781186548,-0.707106781186548));
#6063=DIRECTION('ref_axis',(-1.,0.,0.));
#6064=DIRECTION('',(1.,0.,0.));
#6065=DIRECTION('center_axis',(0.,1.,0.));
#6066=DIRECTION('ref_axis',(-1.,0.,0.));
#6067=DIRECTION('axis',(0.,0.,1.));
#6068=DIRECTION('refdir',(1.,0.,0.));
#6069=DIRECTION('center_axis',(0.866025403784439,0.,-0.5));
#6070=DIRECTION('ref_axis',(0.5,0.,0.866025403784439));
#6071=DIRECTION('',(-0.5,0.,-0.866025403784439));
#6072=DIRECTION('',(0.,-1.,0.));
#6073=DIRECTION('',(0.5,0.,0.866025403784439));
#6074=DIRECTION('',(0.,-1.,0.));
#6075=DIRECTION('center_axis',(1.20185167898973E-16,0.,-1.));
#6076=DIRECTION('ref_axis',(1.,0.,1.20185167898973E-16));
#6077=DIRECTION('',(-1.,0.,-1.20185167898973E-16));
#6078=DIRECTION('',(0.,-1.,0.));
#6079=DIRECTION('',(1.,0.,1.20185167898973E-16));
#6080=DIRECTION('center_axis',(-0.866025403784439,0.,-0.5));
#6081=DIRECTION('ref_axis',(0.5,0.,-0.866025403784439));
#6082=DIRECTION('',(-0.5,0.,0.866025403784439));
#6083=DIRECTION('',(0.,-1.,0.));
#6084=DIRECTION('',(0.5,0.,-0.866025403784439));
#6085=DIRECTION('center_axis',(-0.866025403784439,0.,0.5));
#6086=DIRECTION('ref_axis',(-0.5,0.,-0.866025403784439));
#6087=DIRECTION('',(0.5,0.,0.866025403784439));
#6088=DIRECTION('',(0.,-1.,0.));
#6089=DIRECTION('',(-0.5,0.,-0.866025403784439));
#6090=DIRECTION('center_axis',(-2.40370335797945E-16,0.,1.));
#6091=DIRECTION('ref_axis',(-1.,0.,-2.40370335797945E-16));
#6092=DIRECTION('',(1.,0.,2.40370335797945E-16));
#6093=DIRECTION('',(0.,-1.,0.));
#6094=DIRECTION('',(-1.,0.,-2.40370335797945E-16));
#6095=DIRECTION('center_axis',(0.866025403784439,0.,0.5));
#6096=DIRECTION('ref_axis',(-0.5,0.,0.866025403784439));
#6097=DIRECTION('',(0.5,0.,-0.866025403784439));
#6098=DIRECTION('',(-0.5,0.,0.866025403784439));
#6099=DIRECTION('center_axis',(0.,1.,0.));
#6100=DIRECTION('ref_axis',(1.,0.,0.));
#6101=DIRECTION('center_axis',(0.,-1.,0.));
#6102=DIRECTION('ref_axis',(0.,0.,-1.));
#6103=DIRECTION('center_axis',(0.,1.,0.));
#6104=DIRECTION('ref_axis',(1.,0.,0.));
#6105=DIRECTION('center_axis',(0.,1.,0.));
#6106=DIRECTION('ref_axis',(1.,0.,0.));
#6107=DIRECTION('center_axis',(0.,1.,0.));
#6108=DIRECTION('ref_axis',(0.,0.,1.));
#6109=DIRECTION('center_axis',(0.,-1.,0.));
#6110=DIRECTION('ref_axis',(1.,0.,0.));
#6111=DIRECTION('center_axis',(0.,-1.,0.));
#6112=DIRECTION('ref_axis',(1.,0.,0.));
#6113=DIRECTION('center_axis',(0.,-1.,0.));
#6114=DIRECTION('ref_axis',(1.,0.,0.));
#6115=DIRECTION('',(0.707106781186548,0.707106781186547,8.65956056235493E-17));
#6116=DIRECTION('center_axis',(0.,-1.,0.));
#6117=DIRECTION('ref_axis',(1.,0.,0.));
#6118=DIRECTION('center_axis',(0.,-1.,0.));
#6119=DIRECTION('ref_axis',(1.,0.,0.));
#6120=DIRECTION('',(0.,1.,0.));
#6121=DIRECTION('center_axis',(0.,1.,0.));
#6122=DIRECTION('ref_axis',(1.,0.,0.));
#6123=DIRECTION('center_axis',(0.,-1.,0.));
#6124=DIRECTION('ref_axis',(1.,0.,0.));
#6125=DIRECTION('',(-0.707106781186547,0.707106781186548,-8.65956056235493E-17));
#6126=DIRECTION('center_axis',(0.,-1.,0.));
#6127=DIRECTION('ref_axis',(0.,0.,-1.));
#6128=DIRECTION('center_axis',(0.,-1.,0.));
#6129=DIRECTION('ref_axis',(1.,0.,0.));
#6130=DIRECTION('center_axis',(0.,1.,0.));
#6131=DIRECTION('ref_axis',(1.,0.,0.));
#6132=DIRECTION('center_axis',(0.,1.,0.));
#6133=DIRECTION('ref_axis',(1.,0.,0.));
#6134=DIRECTION('',(-0.447213595499958,0.894427190999916,-5.47678698264203E-17));
#6135=DIRECTION('center_axis',(0.,-1.,0.));
#6136=DIRECTION('ref_axis',(1.,0.,0.));
#6137=DIRECTION('',(0.,1.,0.));
#6138=DIRECTION('axis',(0.,0.,1.));
#6139=DIRECTION('refdir',(1.,0.,0.));
#6140=DIRECTION('center_axis',(0.,0.,1.));
#6141=DIRECTION('ref_axis',(1.,0.,0.));
#6142=DIRECTION('center_axis',(0.,0.,1.));
#6143=DIRECTION('ref_axis',(1.,0.,0.));
#6144=DIRECTION('',(0.,0.,1.));
#6145=DIRECTION('center_axis',(0.,0.,-1.));
#6146=DIRECTION('ref_axis',(1.,0.,0.));
#6147=DIRECTION('center_axis',(0.,0.,1.));
#6148=DIRECTION('ref_axis',(1.,0.,0.));
#6149=DIRECTION('center_axis',(0.,0.,1.));
#6150=DIRECTION('ref_axis',(1.,0.,0.));
#6151=DIRECTION('center_axis',(0.,0.,1.));
#6152=DIRECTION('ref_axis',(1.,0.,0.));
#6153=DIRECTION('center_axis',(0.,0.,1.));
#6154=DIRECTION('ref_axis',(1.,0.,0.));
#6155=DIRECTION('',(0.,0.,1.));
#6156=DIRECTION('center_axis',(0.,0.,-1.));
#6157=DIRECTION('ref_axis',(1.,0.,0.));
#6158=DIRECTION('center_axis',(0.,0.,1.));
#6159=DIRECTION('ref_axis',(1.,0.,0.));
#6160=DIRECTION('center_axis',(0.,0.,1.));
#6161=DIRECTION('ref_axis',(1.,0.,0.));
#6162=DIRECTION('center_axis',(0.,0.,1.));
#6163=DIRECTION('ref_axis',(1.,0.,0.));
#6164=DIRECTION('center_axis',(0.,0.,1.));
#6165=DIRECTION('ref_axis',(1.,0.,0.));
#6166=DIRECTION('',(0.,0.,1.));
#6167=DIRECTION('center_axis',(0.,0.,-1.));
#6168=DIRECTION('ref_axis',(1.,0.,0.));
#6169=DIRECTION('center_axis',(0.,0.,1.));
#6170=DIRECTION('ref_axis',(1.,0.,0.));
#6171=DIRECTION('center_axis',(0.,0.,1.));
#6172=DIRECTION('ref_axis',(1.,0.,0.));
#6173=DIRECTION('center_axis',(0.,0.,1.));
#6174=DIRECTION('ref_axis',(1.,0.,0.));
#6175=DIRECTION('center_axis',(0.,0.,1.));
#6176=DIRECTION('ref_axis',(1.,0.,0.));
#6177=DIRECTION('',(0.,0.,1.));
#6178=DIRECTION('center_axis',(0.,0.,-1.));
#6179=DIRECTION('ref_axis',(1.,0.,0.));
#6180=DIRECTION('center_axis',(0.,0.,1.));
#6181=DIRECTION('ref_axis',(1.,0.,0.));
#6182=DIRECTION('center_axis',(0.,0.,1.));
#6183=DIRECTION('ref_axis',(1.,0.,0.));
#6184=DIRECTION('center_axis',(0.,0.,1.));
#6185=DIRECTION('ref_axis',(1.,0.,0.));
#6186=DIRECTION('center_axis',(0.,0.,1.));
#6187=DIRECTION('ref_axis',(1.,0.,0.));
#6188=DIRECTION('',(0.,0.,1.));
#6189=DIRECTION('center_axis',(0.,0.,1.));
#6190=DIRECTION('ref_axis',(1.,0.,0.));
#6191=DIRECTION('center_axis',(0.,0.,1.));
#6192=DIRECTION('ref_axis',(1.,0.,0.));
#6193=DIRECTION('',(0.,0.,1.));
#6194=DIRECTION('center_axis',(0.,0.,1.));
#6195=DIRECTION('ref_axis',(1.,0.,0.));
#6196=DIRECTION('center_axis',(0.,0.,1.));
#6197=DIRECTION('ref_axis',(1.,0.,0.));
#6198=DIRECTION('',(0.,0.,1.));
#6199=DIRECTION('center_axis',(0.,0.,1.));
#6200=DIRECTION('ref_axis',(1.,0.,0.));
#6201=DIRECTION('center_axis',(0.,0.,1.));
#6202=DIRECTION('ref_axis',(1.,0.,0.));
#6203=DIRECTION('',(0.,0.,1.));
#6204=DIRECTION('center_axis',(0.,-0.56333682464151,0.826227342807548));
#6205=DIRECTION('ref_axis',(0.,-0.826227342807548,-0.56333682464151));
#6206=DIRECTION('',(0.,-0.826227342807548,-0.56333682464151));
#6207=DIRECTION('',(1.,0.,0.));
#6208=DIRECTION('',(0.,-0.826227342807548,-0.56333682464151));
#6209=DIRECTION('',(1.,0.,0.));
#6210=DIRECTION('center_axis',(0.,-1.,0.));
#6211=DIRECTION('ref_axis',(0.,0.,-1.));
#6212=DIRECTION('',(0.,0.,-1.));
#6213=DIRECTION('',(0.,0.,-1.));
#6214=DIRECTION('',(1.,0.,0.));
#6215=DIRECTION('center_axis',(0.,-0.56333682464151,-0.826227342807548));
#6216=DIRECTION('ref_axis',(0.,0.826227342807548,-0.56333682464151));
#6217=DIRECTION('',(0.,0.826227342807548,-0.56333682464151));
#6218=DIRECTION('',(0.,0.826227342807548,-0.56333682464151));
#6219=DIRECTION('',(1.,0.,0.));
#6220=DIRECTION('center_axis',(0.,-1.,0.));
#6221=DIRECTION('ref_axis',(0.,0.,-1.));
#6222=DIRECTION('',(0.,0.,-1.));
#6223=DIRECTION('',(0.,0.,-1.));
#6224=DIRECTION('',(1.,0.,0.));
#6225=DIRECTION('center_axis',(0.,0.,1.));
#6226=DIRECTION('ref_axis',(0.,-1.,0.));
#6227=DIRECTION('',(0.,-1.,0.));
#6228=DIRECTION('',(0.,-1.,0.));
#6229=DIRECTION('',(1.,0.,0.));
#6230=DIRECTION('center_axis',(0.,1.,0.));
#6231=DIRECTION('ref_axis',(0.,0.,1.));
#6232=DIRECTION('',(0.,0.,1.));
#6233=DIRECTION('',(0.,0.,1.));
#6234=DIRECTION('',(1.,0.,0.));
#6235=DIRECTION('center_axis',(0.,0.56333682464151,-0.826227342807548));
#6236=DIRECTION('ref_axis',(0.,0.826227342807548,0.56333682464151));
#6237=DIRECTION('',(0.,0.826227342807548,0.56333682464151));
#6238=DIRECTION('',(0.,0.826227342807548,0.56333682464151));
#6239=DIRECTION('',(1.,0.,0.));
#6240=DIRECTION('center_axis',(0.,1.,0.));
#6241=DIRECTION('ref_axis',(0.,0.,1.));
#6242=DIRECTION('',(0.,0.,1.));
#6243=DIRECTION('',(0.,0.,1.));
#6244=DIRECTION('',(1.,0.,0.));
#6245=DIRECTION('center_axis',(0.,0.56333682464151,0.826227342807548));
#6246=DIRECTION('ref_axis',(0.,-0.826227342807548,0.56333682464151));
#6247=DIRECTION('',(0.,-0.826227342807548,0.56333682464151));
#6248=DIRECTION('',(0.,-0.826227342807548,0.56333682464151));
#6249=DIRECTION('',(1.,0.,0.));
#6250=DIRECTION('center_axis',(0.,1.,0.));
#6251=DIRECTION('ref_axis',(0.,0.,1.));
#6252=DIRECTION('',(0.,0.,1.));
#6253=DIRECTION('',(0.,0.,1.));
#6254=DIRECTION('',(1.,0.,0.));
#6255=DIRECTION('center_axis',(0.,0.,-1.));
#6256=DIRECTION('ref_axis',(0.,1.,0.));
#6257=DIRECTION('',(0.,1.,0.));
#6258=DIRECTION('',(0.,1.,0.));
#6259=DIRECTION('',(1.,0.,0.));
#6260=DIRECTION('center_axis',(0.,-1.,0.));
#6261=DIRECTION('ref_axis',(0.,0.,-1.));
#6262=DIRECTION('',(0.,0.,-1.));
#6263=DIRECTION('',(0.,0.,-1.));
#6264=DIRECTION('center_axis',(1.,0.,0.));
#6265=DIRECTION('ref_axis',(0.,0.,-1.));
#6266=DIRECTION('center_axis',(1.,0.,0.));
#6267=DIRECTION('ref_axis',(0.,0.,-1.));
#6268=DIRECTION('axis',(0.,0.,1.));
#6269=DIRECTION('refdir',(1.,0.,0.));
#6270=DIRECTION('center_axis',(0.,1.,0.));
#6271=DIRECTION('ref_axis',(0.,0.,1.));
#6272=DIRECTION('center_axis',(0.,-1.,0.));
#6273=DIRECTION('ref_axis',(1.,0.,0.));
#6274=DIRECTION('center_axis',(0.,-1.,0.));
#6275=DIRECTION('ref_axis',(1.,0.,0.));
#6276=DIRECTION('center_axis',(0.,-1.,0.));
#6277=DIRECTION('ref_axis',(1.,0.,0.));
#6278=DIRECTION('',(0.707106781186547,0.707106781186548,8.65956056235493E-17));
#6279=DIRECTION('center_axis',(0.,-1.,0.));
#6280=DIRECTION('ref_axis',(1.,0.,0.));
#6281=DIRECTION('center_axis',(0.,-1.,0.));
#6282=DIRECTION('ref_axis',(1.,0.,0.));
#6283=DIRECTION('',(0.,1.,0.));
#6284=DIRECTION('center_axis',(0.,1.,0.));
#6285=DIRECTION('ref_axis',(1.,0.,0.));
#6286=DIRECTION('center_axis',(0.,-1.,0.));
#6287=DIRECTION('ref_axis',(1.,0.,0.));
#6288=DIRECTION('',(-0.707106781186547,0.707106781186548,-8.65956056235493E-17));
#6289=DIRECTION('center_axis',(0.,-1.,0.));
#6290=DIRECTION('ref_axis',(0.,0.,-1.));
#6291=DIRECTION('center_axis',(0.,-1.,0.));
#6292=DIRECTION('ref_axis',(1.,0.,0.));
#6293=DIRECTION('center_axis',(0.,1.,0.));
#6294=DIRECTION('ref_axis',(1.,0.,0.));
#6295=DIRECTION('center_axis',(0.,1.,0.));
#6296=DIRECTION('ref_axis',(1.,0.,0.));
#6297=DIRECTION('',(-0.447213595499958,0.894427190999916,-5.47678698264203E-17));
#6298=DIRECTION('center_axis',(0.,-1.,0.));
#6299=DIRECTION('ref_axis',(1.,0.,0.));
#6300=DIRECTION('center_axis',(0.,1.,0.));
#6301=DIRECTION('ref_axis',(1.,0.,0.));
#6302=DIRECTION('',(0.,1.,0.));
#6303=DIRECTION('center_axis',(0.,1.,0.));
#6304=DIRECTION('ref_axis',(1.,0.,0.));
#6305=DIRECTION('center_axis',(0.,-1.,0.));
#6306=DIRECTION('ref_axis',(1.,0.,0.));
#6307=DIRECTION('',(-0.707106781186547,0.707106781186548,-8.65956056235493E-17));
#6308=DIRECTION('center_axis',(0.,-1.,0.));
#6309=DIRECTION('ref_axis',(0.,0.,-1.));
#6310=DIRECTION('center_axis',(0.866025403784439,0.,-0.5));
#6311=DIRECTION('ref_axis',(0.5,0.,0.866025403784439));
#6312=DIRECTION('',(-0.5,0.,-0.866025403784439));
#6313=DIRECTION('',(0.,-1.,0.));
#6314=DIRECTION('',(0.5,0.,0.866025403784439));
#6315=DIRECTION('',(0.,-1.,0.));
#6316=DIRECTION('center_axis',(1.60246890531964E-16,0.,-1.));
#6317=DIRECTION('ref_axis',(1.,0.,1.60246890531964E-16));
#6318=DIRECTION('',(-1.,0.,-1.60246890531964E-16));
#6319=DIRECTION('',(0.,-1.,0.));
#6320=DIRECTION('',(1.,0.,1.60246890531964E-16));
#6321=DIRECTION('center_axis',(-0.866025403784439,0.,-0.5));
#6322=DIRECTION('ref_axis',(0.5,0.,-0.866025403784439));
#6323=DIRECTION('',(-0.5,0.,0.866025403784439));
#6324=DIRECTION('',(0.,-1.,0.));
#6325=DIRECTION('',(0.5,0.,-0.866025403784439));
#6326=DIRECTION('center_axis',(-0.866025403784439,0.,0.5));
#6327=DIRECTION('ref_axis',(-0.5,0.,-0.866025403784439));
#6328=DIRECTION('',(0.5,0.,0.866025403784439));
#6329=DIRECTION('',(0.,-1.,0.));
#6330=DIRECTION('',(-0.5,0.,-0.866025403784439));
#6331=DIRECTION('center_axis',(-1.60246890531964E-16,0.,1.));
#6332=DIRECTION('ref_axis',(-1.,0.,-1.60246890531964E-16));
#6333=DIRECTION('',(1.,0.,1.60246890531964E-16));
#6334=DIRECTION('',(0.,-1.,0.));
#6335=DIRECTION('',(-1.,0.,-1.60246890531964E-16));
#6336=DIRECTION('center_axis',(0.866025403784439,0.,0.5));
#6337=DIRECTION('ref_axis',(-0.5,0.,0.866025403784439));
#6338=DIRECTION('',(0.5,0.,-0.866025403784439));
#6339=DIRECTION('',(-0.5,0.,0.866025403784439));
#6340=DIRECTION('center_axis',(0.,1.,0.));
#6341=DIRECTION('ref_axis',(1.,0.,0.));
#6342=DIRECTION('center_axis',(0.,-1.,0.));
#6343=DIRECTION('ref_axis',(0.,0.,-1.));
#6344=DIRECTION('axis',(0.,0.,1.));
#6345=DIRECTION('refdir',(1.,0.,0.));
#6346=DIRECTION('center_axis',(0.,0.,1.));
#6347=DIRECTION('ref_axis',(1.,0.,0.));
#6348=DIRECTION('center_axis',(0.,0.,1.));
#6349=DIRECTION('ref_axis',(1.,0.,0.));
#6350=DIRECTION('',(0.,0.,1.));
#6351=DIRECTION('center_axis',(0.,0.,-1.));
#6352=DIRECTION('ref_axis',(1.,0.,0.));
#6353=DIRECTION('center_axis',(0.,0.,1.));
#6354=DIRECTION('ref_axis',(1.,0.,0.));
#6355=DIRECTION('center_axis',(0.,0.,1.));
#6356=DIRECTION('ref_axis',(1.,0.,0.));
#6357=DIRECTION('center_axis',(0.,0.,1.));
#6358=DIRECTION('ref_axis',(1.,0.,0.));
#6359=DIRECTION('center_axis',(0.,0.,1.));
#6360=DIRECTION('ref_axis',(1.,0.,0.));
#6361=DIRECTION('',(0.,0.,1.));
#6362=DIRECTION('center_axis',(0.,0.,-1.));
#6363=DIRECTION('ref_axis',(1.,0.,0.));
#6364=DIRECTION('center_axis',(0.,0.,1.));
#6365=DIRECTION('ref_axis',(1.,0.,0.));
#6366=DIRECTION('center_axis',(0.,0.,1.));
#6367=DIRECTION('ref_axis',(1.,0.,0.));
#6368=DIRECTION('center_axis',(0.,0.,1.));
#6369=DIRECTION('ref_axis',(1.,0.,0.));
#6370=DIRECTION('center_axis',(0.,0.,1.));
#6371=DIRECTION('ref_axis',(1.,0.,0.));
#6372=DIRECTION('',(0.,0.,1.));
#6373=DIRECTION('center_axis',(0.,0.,1.));
#6374=DIRECTION('ref_axis',(1.,0.,0.));
#6375=DIRECTION('center_axis',(0.,0.,1.));
#6376=DIRECTION('ref_axis',(1.,0.,0.));
#6377=DIRECTION('',(0.,0.,1.));
#6378=DIRECTION('center_axis',(0.,1.,0.));
#6379=DIRECTION('ref_axis',(-1.,0.,0.));
#6380=DIRECTION('',(-1.,0.,0.));
#6381=DIRECTION('',(0.,0.,1.));
#6382=DIRECTION('',(-1.,0.,0.));
#6383=DIRECTION('',(0.,0.,1.));
#6384=DIRECTION('center_axis',(1.,0.,0.));
#6385=DIRECTION('ref_axis',(0.,1.,0.));
#6386=DIRECTION('',(0.,1.,0.));
#6387=DIRECTION('',(0.,1.,0.));
#6388=DIRECTION('',(0.,0.,1.));
#6389=DIRECTION('center_axis',(0.,-1.,0.));
#6390=DIRECTION('ref_axis',(1.,0.,0.));
#6391=DIRECTION('',(1.,0.,0.));
#6392=DIRECTION('',(1.,0.,0.));
#6393=DIRECTION('',(0.,0.,1.));
#6394=DIRECTION('center_axis',(-1.,0.,0.));
#6395=DIRECTION('ref_axis',(0.,-1.,0.));
#6396=DIRECTION('',(0.,-1.,0.));
#6397=DIRECTION('',(0.,-1.,0.));
#6398=DIRECTION('center_axis',(0.,0.,1.));
#6399=DIRECTION('ref_axis',(1.,0.,0.));
#6400=DIRECTION('center_axis',(0.,0.,1.));
#6401=DIRECTION('ref_axis',(1.,0.,0.));
#6402=DIRECTION('axis',(0.,0.,1.));
#6403=DIRECTION('refdir',(1.,0.,0.));
#6404=DIRECTION('center_axis',(0.,1.,0.));
#6405=DIRECTION('ref_axis',(-1.,0.,0.));
#6406=DIRECTION('',(-1.,0.,0.));
#6407=DIRECTION('',(0.,0.,1.));
#6408=DIRECTION('',(-1.,0.,0.));
#6409=DIRECTION('',(0.,0.,1.));
#6410=DIRECTION('center_axis',(1.,0.,0.));
#6411=DIRECTION('ref_axis',(0.,1.,0.));
#6412=DIRECTION('',(0.,1.,0.));
#6413=DIRECTION('',(0.,1.,0.));
#6414=DIRECTION('',(0.,0.,1.));
#6415=DIRECTION('center_axis',(0.,-1.,0.));
#6416=DIRECTION('ref_axis',(1.,0.,0.));
#6417=DIRECTION('',(1.,0.,0.));
#6418=DIRECTION('',(1.,0.,0.));
#6419=DIRECTION('',(0.,0.,1.));
#6420=DIRECTION('center_axis',(-1.,0.,0.));
#6421=DIRECTION('ref_axis',(0.,-1.,0.));
#6422=DIRECTION('',(0.,-1.,0.));
#6423=DIRECTION('',(0.,-1.,0.));
#6424=DIRECTION('center_axis',(0.,0.,1.));
#6425=DIRECTION('ref_axis',(1.,0.,0.));
#6426=DIRECTION('center_axis',(0.,0.,1.));
#6427=DIRECTION('ref_axis',(1.,0.,0.));
#6428=DIRECTION('axis',(0.,0.,1.));
#6429=DIRECTION('refdir',(1.,0.,0.));
#6430=DIRECTION('center_axis',(0.,1.,0.));
#6431=DIRECTION('ref_axis',(-1.,0.,0.));
#6432=DIRECTION('',(-1.,0.,0.));
#6433=DIRECTION('',(0.,0.,1.));
#6434=DIRECTION('',(-1.,0.,0.));
#6435=DIRECTION('',(0.,0.,1.));
#6436=DIRECTION('center_axis',(1.,0.,0.));
#6437=DIRECTION('ref_axis',(0.,1.,0.));
#6438=DIRECTION('',(0.,1.,0.));
#6439=DIRECTION('',(0.,1.,0.));
#6440=DIRECTION('',(0.,0.,1.));
#6441=DIRECTION('center_axis',(0.,-1.,0.));
#6442=DIRECTION('ref_axis',(1.,0.,0.));
#6443=DIRECTION('',(1.,0.,0.));
#6444=DIRECTION('',(1.,0.,0.));
#6445=DIRECTION('',(0.,0.,1.));
#6446=DIRECTION('center_axis',(-1.,0.,0.));
#6447=DIRECTION('ref_axis',(0.,-1.,0.));
#6448=DIRECTION('',(0.,-1.,0.));
#6449=DIRECTION('',(0.,-1.,0.));
#6450=DIRECTION('center_axis',(0.,0.,1.));
#6451=DIRECTION('ref_axis',(1.,0.,0.));
#6452=DIRECTION('center_axis',(0.,0.,1.));
#6453=DIRECTION('ref_axis',(1.,0.,0.));
#6454=DIRECTION('axis',(0.,0.,1.));
#6455=DIRECTION('refdir',(1.,0.,0.));
#6456=DIRECTION('axis',(0.,0.,1.));
#6457=DIRECTION('refdir',(1.,0.,0.));
#6458=DIRECTION('axis',(0.,0.,1.));
#6459=DIRECTION('refdir',(1.,0.,0.));
#6460=DIRECTION('center_axis',(0.,0.,1.));
#6461=DIRECTION('ref_axis',(1.,0.,0.));
#6462=DIRECTION('',(-1.,0.,0.));
#6463=DIRECTION('center_axis',(0.,0.,1.));
#6464=DIRECTION('ref_axis',(1.,0.,0.));
#6465=DIRECTION('center_axis',(0.,0.,1.));
#6466=DIRECTION('ref_axis',(1.,0.,0.));
#6467=DIRECTION('',(0.,0.,-1.));
#6468=DIRECTION('center_axis',(0.,0.,1.));
#6469=DIRECTION('ref_axis',(1.,0.,0.));
#6470=DIRECTION('',(0.,0.,1.));
#6471=DIRECTION('center_axis',(0.,0.,-1.));
#6472=DIRECTION('ref_axis',(1.,0.,0.));
#6473=DIRECTION('center_axis',(0.,0.,1.));
#6474=DIRECTION('ref_axis',(1.,0.,0.));
#6475=DIRECTION('',(0.,0.,1.));
#6476=DIRECTION('center_axis',(0.,0.,1.));
#6477=DIRECTION('ref_axis',(1.,0.,0.));
#6478=DIRECTION('',(1.,0.,0.));
#6479=DIRECTION('center_axis',(0.,0.,1.));
#6480=DIRECTION('ref_axis',(1.,0.,0.));
#6481=DIRECTION('center_axis',(0.,0.,1.));
#6482=DIRECTION('ref_axis',(1.,0.,0.));
#6483=DIRECTION('',(0.,0.,-1.));
#6484=DIRECTION('center_axis',(0.,0.,1.));
#6485=DIRECTION('ref_axis',(1.,0.,0.));
#6486=DIRECTION('',(0.,0.,1.));
#6487=DIRECTION('center_axis',(0.,0.,-1.));
#6488=DIRECTION('ref_axis',(1.,0.,0.));
#6489=DIRECTION('center_axis',(0.,0.,1.));
#6490=DIRECTION('ref_axis',(1.,0.,0.));
#6491=DIRECTION('',(0.,0.,1.));
#6492=DIRECTION('center_axis',(0.,0.,1.));
#6493=DIRECTION('ref_axis',(1.,0.,0.));
#6494=DIRECTION('',(-1.,0.,0.));
#6495=DIRECTION('center_axis',(0.,0.,1.));
#6496=DIRECTION('ref_axis',(1.,0.,0.));
#6497=DIRECTION('center_axis',(0.,0.,1.));
#6498=DIRECTION('ref_axis',(1.,0.,0.));
#6499=DIRECTION('',(0.,0.,-1.));
#6500=DIRECTION('center_axis',(0.,0.,1.));
#6501=DIRECTION('ref_axis',(1.,0.,0.));
#6502=DIRECTION('',(0.,0.,1.));
#6503=DIRECTION('center_axis',(0.,0.,-1.));
#6504=DIRECTION('ref_axis',(1.,0.,0.));
#6505=DIRECTION('center_axis',(0.,0.,1.));
#6506=DIRECTION('ref_axis',(1.,0.,0.));
#6507=DIRECTION('',(0.,0.,1.));
#6508=DIRECTION('center_axis',(0.,0.,1.));
#6509=DIRECTION('ref_axis',(1.,0.,0.));
#6510=DIRECTION('',(1.,0.,0.));
#6511=DIRECTION('center_axis',(0.,0.,1.));
#6512=DIRECTION('ref_axis',(1.,0.,0.));
#6513=DIRECTION('center_axis',(0.,0.,1.));
#6514=DIRECTION('ref_axis',(1.,0.,0.));
#6515=DIRECTION('',(0.,0.,-1.));
#6516=DIRECTION('center_axis',(0.,0.,1.));
#6517=DIRECTION('ref_axis',(1.,0.,0.));
#6518=DIRECTION('',(0.,0.,1.));
#6519=DIRECTION('center_axis',(0.,0.,-1.));
#6520=DIRECTION('ref_axis',(1.,0.,0.));
#6521=DIRECTION('center_axis',(0.,0.,1.));
#6522=DIRECTION('ref_axis',(1.,0.,0.));
#6523=DIRECTION('',(0.,0.,1.));
#6524=DIRECTION('center_axis',(0.,-1.,0.));
#6525=DIRECTION('ref_axis',(0.,0.,-1.));
#6526=DIRECTION('',(-1.,0.,0.));
#6527=DIRECTION('',(-1.,0.,0.));
#6528=DIRECTION('',(0.,0.,1.));
#6529=DIRECTION('',(1.,0.,0.));
#6530=DIRECTION('',(0.,0.,-1.));
#6531=DIRECTION('',(-1.,0.,0.));
#6532=DIRECTION('center_axis',(0.,1.,0.));
#6533=DIRECTION('ref_axis',(0.,0.,1.));
#6534=DIRECTION('',(1.,0.,0.));
#6535=DIRECTION('',(1.,0.,0.));
#6536=DIRECTION('',(0.,0.,1.));
#6537=DIRECTION('',(1.,0.,0.));
#6538=DIRECTION('',(0.,0.,-1.));
#6539=DIRECTION('',(1.,0.,0.));
#6540=DIRECTION('center_axis',(-1.,0.,0.));
#6541=DIRECTION('ref_axis',(0.,0.,1.));
#6542=DIRECTION('',(0.,-1.,0.));
#6543=DIRECTION('',(0.,0.,1.));
#6544=DIRECTION('',(0.,1.,0.));
#6545=DIRECTION('',(0.,0.,-1.));
#6546=DIRECTION('',(0.,-1.,0.));
#6547=DIRECTION('',(0.,-1.,0.));
#6548=DIRECTION('',(0.,0.,1.));
#6549=DIRECTION('',(0.,-1.,0.));
#6550=DIRECTION('',(0.,0.,-1.));
#6551=DIRECTION('',(0.,-1.,0.));
#6552=DIRECTION('center_axis',(0.,0.,-1.));
#6553=DIRECTION('ref_axis',(0.,1.,0.));
#6554=DIRECTION('',(0.,1.,0.));
#6555=DIRECTION('',(1.,0.,0.));
#6556=DIRECTION('center_axis',(0.,-1.,0.));
#6557=DIRECTION('ref_axis',(0.,0.,-1.));
#6558=DIRECTION('',(0.,0.,-1.));
#6559=DIRECTION('',(1.,0.,0.));
#6560=DIRECTION('center_axis',(0.,0.,1.));
#6561=DIRECTION('ref_axis',(0.,-1.,0.));
#6562=DIRECTION('',(0.,-1.,0.));
#6563=DIRECTION('',(1.,0.,0.));
#6564=DIRECTION('center_axis',(0.,1.,0.));
#6565=DIRECTION('ref_axis',(0.,0.,1.));
#6566=DIRECTION('',(0.,0.,1.));
#6567=DIRECTION('',(1.,0.,0.));
#6568=DIRECTION('center_axis',(0.,0.,-1.));
#6569=DIRECTION('ref_axis',(0.,1.,0.));
#6570=DIRECTION('',(0.,1.,0.));
#6571=DIRECTION('center_axis',(0.,0.,-1.));
#6572=DIRECTION('ref_axis',(0.,1.,0.));
#6573=DIRECTION('',(0.,1.,0.));
#6574=DIRECTION('',(1.,0.,0.));
#6575=DIRECTION('center_axis',(0.,-1.,0.));
#6576=DIRECTION('ref_axis',(0.,0.,-1.));
#6577=DIRECTION('',(0.,0.,-1.));
#6578=DIRECTION('',(1.,0.,0.));
#6579=DIRECTION('center_axis',(0.,0.,-1.));
#6580=DIRECTION('ref_axis',(0.,1.,0.));
#6581=DIRECTION('',(0.,1.,0.));
#6582=DIRECTION('',(1.,0.,0.));
#6583=DIRECTION('center_axis',(0.,1.,0.));
#6584=DIRECTION('ref_axis',(0.,0.,1.));
#6585=DIRECTION('',(0.,0.,1.));
#6586=DIRECTION('',(1.,0.,0.));
#6587=DIRECTION('center_axis',(0.,0.,-1.));
#6588=DIRECTION('ref_axis',(0.,1.,0.));
#6589=DIRECTION('',(0.,1.,0.));
#6590=DIRECTION('center_axis',(1.,0.,0.));
#6591=DIRECTION('ref_axis',(0.,0.,-1.));
#6592=DIRECTION('axis',(0.,0.,1.));
#6593=DIRECTION('refdir',(1.,0.,0.));
#6594=DIRECTION('center_axis',(0.,0.,1.));
#6595=DIRECTION('ref_axis',(0.,-1.,0.));
#6596=DIRECTION('',(0.,-1.,0.));
#6597=DIRECTION('',(1.,0.,0.));
#6598=DIRECTION('',(0.,-1.,0.));
#6599=DIRECTION('',(1.,0.,0.));
#6600=DIRECTION('center_axis',(0.,1.,0.));
#6601=DIRECTION('ref_axis',(0.,0.,1.));
#6602=DIRECTION('',(0.,0.,1.));
#6603=DIRECTION('',(0.,0.,1.));
#6604=DIRECTION('',(1.,0.,0.));
#6605=DIRECTION('center_axis',(0.,0.,-1.));
#6606=DIRECTION('ref_axis',(0.,1.,0.));
#6607=DIRECTION('',(0.,1.,0.));
#6608=DIRECTION('',(0.,1.,0.));
#6609=DIRECTION('',(1.,0.,0.));
#6610=DIRECTION('center_axis',(0.,-1.,0.));
#6611=DIRECTION('ref_axis',(0.,0.,-1.));
#6612=DIRECTION('',(0.,0.,-1.));
#6613=DIRECTION('',(0.,0.,-1.));
#6614=DIRECTION('',(1.,0.,0.));
#6615=DIRECTION('center_axis',(0.,0.,-1.));
#6616=DIRECTION('ref_axis',(0.,1.,0.));
#6617=DIRECTION('',(0.,1.,0.));
#6618=DIRECTION('',(0.,1.,0.));
#6619=DIRECTION('',(1.,0.,0.));
#6620=DIRECTION('center_axis',(0.,1.,0.));
#6621=DIRECTION('ref_axis',(0.,0.,1.));
#6622=DIRECTION('',(0.,0.,1.));
#6623=DIRECTION('',(0.,0.,1.));
#6624=DIRECTION('',(1.,0.,0.));
#6625=DIRECTION('center_axis',(0.,0.,-1.));
#6626=DIRECTION('ref_axis',(0.,1.,0.));
#6627=DIRECTION('',(0.,1.,0.));
#6628=DIRECTION('',(0.,1.,0.));
#6629=DIRECTION('',(1.,0.,0.));
#6630=DIRECTION('center_axis',(0.,-1.,0.));
#6631=DIRECTION('ref_axis',(0.,0.,-1.));
#6632=DIRECTION('',(0.,0.,-1.));
#6633=DIRECTION('',(0.,0.,-1.));
#6634=DIRECTION('center_axis',(1.,0.,0.));
#6635=DIRECTION('ref_axis',(0.,0.,-1.));
#6636=DIRECTION('center_axis',(1.,0.,0.));
#6637=DIRECTION('ref_axis',(0.,0.,-1.));
#6638=DIRECTION('axis',(0.,0.,1.));
#6639=DIRECTION('refdir',(1.,0.,0.));
#6640=DIRECTION('center_axis',(0.,0.,-1.));
#6641=DIRECTION('ref_axis',(0.,-1.,0.));
#6642=DIRECTION('',(0.,1.,0.));
#6643=DIRECTION('',(-1.,0.,0.));
#6644=DIRECTION('',(0.,-1.,0.));
#6645=DIRECTION('',(-1.,0.,0.));
#6646=DIRECTION('center_axis',(0.,1.,0.));
#6647=DIRECTION('ref_axis',(0.,0.,-1.));
#6648=DIRECTION('',(0.,0.,1.));
#6649=DIRECTION('',(0.,0.,-1.));
#6650=DIRECTION('',(-1.,0.,0.));
#6651=DIRECTION('center_axis',(0.,0.,-1.));
#6652=DIRECTION('ref_axis',(0.,-1.,0.));
#6653=DIRECTION('',(0.,1.,0.));
#6654=DIRECTION('',(0.,-1.,0.));
#6655=DIRECTION('',(-1.,0.,0.));
#6656=DIRECTION('center_axis',(0.,-1.,0.));
#6657=DIRECTION('ref_axis',(0.,0.,1.));
#6658=DIRECTION('',(0.,0.,-1.));
#6659=DIRECTION('',(0.,0.,1.));
#6660=DIRECTION('',(-1.,0.,0.));
#6661=DIRECTION('center_axis',(0.,0.,-1.));
#6662=DIRECTION('ref_axis',(0.,-1.,0.));
#6663=DIRECTION('',(0.,1.,0.));
#6664=DIRECTION('',(0.,-1.,0.));
#6665=DIRECTION('',(-1.,0.,0.));
#6666=DIRECTION('center_axis',(0.,1.,0.));
#6667=DIRECTION('ref_axis',(0.,0.,-1.));
#6668=DIRECTION('',(0.,0.,1.));
#6669=DIRECTION('',(0.,0.,-1.));
#6670=DIRECTION('',(-1.,0.,0.));
#6671=DIRECTION('center_axis',(0.,0.,1.));
#6672=DIRECTION('ref_axis',(0.,1.,0.));
#6673=DIRECTION('',(0.,-1.,0.));
#6674=DIRECTION('',(0.,1.,0.));
#6675=DIRECTION('',(-1.,0.,0.));
#6676=DIRECTION('center_axis',(0.,-1.,0.));
#6677=DIRECTION('ref_axis',(0.,0.,1.));
#6678=DIRECTION('',(0.,0.,-1.));
#6679=DIRECTION('',(0.,0.,1.));
#6680=DIRECTION('center_axis',(1.,0.,0.));
#6681=DIRECTION('ref_axis',(0.,0.,-1.));
#6682=DIRECTION('center_axis',(-1.,0.,0.));
#6683=DIRECTION('ref_axis',(0.,0.,1.));
#6684=DIRECTION('',(0.,0.,1.));
#6685=DIRECTION('',(1.,0.,0.));
#6686=DIRECTION('',(0.,0.,1.));
#6687=DIRECTION('',(1.,0.,0.));
#6688=DIRECTION('',(0.,0.,1.));
#6689=DIRECTION('',(1.,0.,0.));
#6690=DIRECTION('axis',(0.,0.,1.));
#6691=DIRECTION('refdir',(1.,0.,0.));
#6692=DIRECTION('center_axis',(0.,0.,1.));
#6693=DIRECTION('ref_axis',(1.,0.,0.));
#6694=DIRECTION('center_axis',(0.,0.,1.));
#6695=DIRECTION('ref_axis',(1.,0.,0.));
#6696=DIRECTION('',(0.,0.,1.));
#6697=DIRECTION('center_axis',(0.,0.,-1.));
#6698=DIRECTION('ref_axis',(1.,0.,0.));
#6699=DIRECTION('center_axis',(0.,0.,1.));
#6700=DIRECTION('ref_axis',(1.,0.,0.));
#6701=DIRECTION('center_axis',(0.,0.,1.));
#6702=DIRECTION('ref_axis',(1.,0.,0.));
#6703=DIRECTION('',(0.,0.,1.));
#6704=DIRECTION('center_axis',(0.,0.,-1.));
#6705=DIRECTION('ref_axis',(1.,0.,0.));
#6706=DIRECTION('center_axis',(0.,0.,1.));
#6707=DIRECTION('ref_axis',(1.,0.,0.));
#6708=DIRECTION('center_axis',(0.,0.,1.));
#6709=DIRECTION('ref_axis',(1.,0.,0.));
#6710=DIRECTION('',(0.,0.,1.));
#6711=DIRECTION('center_axis',(0.,0.,-1.));
#6712=DIRECTION('ref_axis',(1.,0.,0.));
#6713=DIRECTION('center_axis',(0.,0.,1.));
#6714=DIRECTION('ref_axis',(1.,0.,0.));
#6715=DIRECTION('center_axis',(0.,0.,1.));
#6716=DIRECTION('ref_axis',(1.,0.,0.));
#6717=DIRECTION('',(0.,0.,1.));
#6718=DIRECTION('center_axis',(0.,0.,-1.));
#6719=DIRECTION('ref_axis',(1.,0.,0.));
#6720=DIRECTION('center_axis',(0.,0.,1.));
#6721=DIRECTION('ref_axis',(1.,0.,0.));
#6722=DIRECTION('center_axis',(0.,0.,1.));
#6723=DIRECTION('ref_axis',(1.,0.,0.));
#6724=DIRECTION('',(0.,0.,1.));
#6725=DIRECTION('center_axis',(0.,0.,-1.));
#6726=DIRECTION('ref_axis',(1.,0.,0.));
#6727=DIRECTION('center_axis',(0.,0.,1.));
#6728=DIRECTION('ref_axis',(1.,0.,0.));
#6729=DIRECTION('center_axis',(0.,0.,1.));
#6730=DIRECTION('ref_axis',(1.,0.,0.));
#6731=DIRECTION('',(0.,0.,1.));
#6732=DIRECTION('center_axis',(0.,0.,-1.));
#6733=DIRECTION('ref_axis',(1.,0.,0.));
#6734=DIRECTION('center_axis',(0.,1.,0.));
#6735=DIRECTION('ref_axis',(-1.,0.,0.));
#6736=DIRECTION('',(-1.,0.,0.));
#6737=DIRECTION('',(0.,0.,1.));
#6738=DIRECTION('',(-1.,0.,0.));
#6739=DIRECTION('',(0.,0.,1.));
#6740=DIRECTION('center_axis',(1.,0.,0.));
#6741=DIRECTION('ref_axis',(0.,1.,0.));
#6742=DIRECTION('',(0.,1.,0.));
#6743=DIRECTION('',(0.,1.,0.));
#6744=DIRECTION('',(0.,0.,1.));
#6745=DIRECTION('center_axis',(0.,-1.,0.));
#6746=DIRECTION('ref_axis',(1.,0.,0.));
#6747=DIRECTION('',(1.,0.,0.));
#6748=DIRECTION('',(1.,0.,0.));
#6749=DIRECTION('',(0.,0.,1.));
#6750=DIRECTION('center_axis',(-1.,0.,0.));
#6751=DIRECTION('ref_axis',(0.,-1.,0.));
#6752=DIRECTION('',(0.,-1.,0.));
#6753=DIRECTION('',(0.,-1.,0.));
#6754=DIRECTION('center_axis',(0.,0.,1.));
#6755=DIRECTION('ref_axis',(1.,0.,0.));
#6756=DIRECTION('center_axis',(0.,0.,1.));
#6757=DIRECTION('ref_axis',(1.,0.,0.));
#6758=DIRECTION('axis',(0.,0.,1.));
#6759=DIRECTION('refdir',(1.,0.,0.));
#6760=DIRECTION('center_axis',(0.,0.,1.));
#6761=DIRECTION('ref_axis',(1.,0.,0.));
#6762=DIRECTION('center_axis',(0.,0.,-1.));
#6763=DIRECTION('ref_axis',(1.,0.,0.));
#6764=DIRECTION('',(0.,0.,-1.));
#6765=DIRECTION('center_axis',(0.,0.,-1.));
#6766=DIRECTION('ref_axis',(1.,0.,0.));
#6767=DIRECTION('center_axis',(0.,0.,1.));
#6768=DIRECTION('ref_axis',(1.,0.,0.));
#6769=DIRECTION('center_axis',(0.,0.,1.));
#6770=DIRECTION('ref_axis',(1.,0.,0.));
#6771=DIRECTION('',(0.,0.,-1.));
#6772=DIRECTION('center_axis',(0.,0.,1.));
#6773=DIRECTION('ref_axis',(1.,0.,0.));
#6774=DIRECTION('center_axis',(0.,0.,1.));
#6775=DIRECTION('ref_axis',(1.,0.,0.));
#6776=DIRECTION('center_axis',(0.,0.,1.));
#6777=DIRECTION('ref_axis',(1.,0.,0.));
#6778=DIRECTION('axis',(0.,0.,1.));
#6779=DIRECTION('refdir',(1.,0.,0.));
#6780=DIRECTION('center_axis',(0.,1.,0.));
#6781=DIRECTION('ref_axis',(1.,0.,0.));
#6782=DIRECTION('center_axis',(0.,1.,0.));
#6783=DIRECTION('ref_axis',(1.,0.,0.));
#6784=DIRECTION('',(0.707106781186548,-0.707106781186547,-8.65956056235494E-17));
#6785=DIRECTION('center_axis',(0.,-1.,0.));
#6786=DIRECTION('ref_axis',(1.,0.,0.));
#6787=DIRECTION('center_axis',(0.,1.,0.));
#6788=DIRECTION('ref_axis',(1.,0.,0.));
#6789=DIRECTION('',(0.,-1.,0.));
#6790=DIRECTION('center_axis',(0.,-1.,0.));
#6791=DIRECTION('ref_axis',(1.,0.,0.));
#6792=DIRECTION('center_axis',(0.,1.,0.));
#6793=DIRECTION('ref_axis',(1.,0.,0.));
#6794=DIRECTION('center_axis',(0.,1.,0.));
#6795=DIRECTION('ref_axis',(1.,0.,0.));
#6796=DIRECTION('center_axis',(0.,1.,0.));
#6797=DIRECTION('ref_axis',(1.,0.,0.));
#6798=DIRECTION('',(0.,-1.,0.));
#6799=DIRECTION('center_axis',(0.,1.,0.));
#6800=DIRECTION('ref_axis',(1.,0.,0.));
#6801=DIRECTION('center_axis',(0.,1.,0.));
#6802=DIRECTION('ref_axis',(1.,0.,0.));
#6803=DIRECTION('axis',(0.,0.,1.));
#6804=DIRECTION('refdir',(1.,0.,0.));
#6805=DIRECTION('center_axis',(0.,1.,0.));
#6806=DIRECTION('ref_axis',(0.,0.,1.));
#6807=DIRECTION('center_axis',(0.,-1.,0.));
#6808=DIRECTION('ref_axis',(1.,0.,0.));
#6809=DIRECTION('center_axis',(0.,-1.,0.));
#6810=DIRECTION('ref_axis',(1.,0.,0.));
#6811=DIRECTION('center_axis',(0.,-1.,0.));
#6812=DIRECTION('ref_axis',(1.,0.,0.));
#6813=DIRECTION('',(0.707106781186548,0.707106781186547,8.65956056235493E-17));
#6814=DIRECTION('center_axis',(0.,-1.,0.));
#6815=DIRECTION('ref_axis',(1.,0.,0.));
#6816=DIRECTION('center_axis',(0.,-1.,0.));
#6817=DIRECTION('ref_axis',(1.,0.,0.));
#6818=DIRECTION('',(0.,1.,0.));
#6819=DIRECTION('center_axis',(0.,1.,0.));
#6820=DIRECTION('ref_axis',(1.,0.,0.));
#6821=DIRECTION('center_axis',(0.,-1.,0.));
#6822=DIRECTION('ref_axis',(1.,0.,0.));
#6823=DIRECTION('',(-0.707106781186547,0.707106781186548,-8.65956056235493E-17));
#6824=DIRECTION('center_axis',(0.,-1.,0.));
#6825=DIRECTION('ref_axis',(0.,0.,-1.));
#6826=DIRECTION('center_axis',(0.,-1.,0.));
#6827=DIRECTION('ref_axis',(1.,0.,0.));
#6828=DIRECTION('center_axis',(0.,1.,0.));
#6829=DIRECTION('ref_axis',(1.,0.,0.));
#6830=DIRECTION('center_axis',(0.,1.,0.));
#6831=DIRECTION('ref_axis',(1.,0.,0.));
#6832=DIRECTION('',(-0.447213595499958,0.894427190999916,-5.47678698264203E-17));
#6833=DIRECTION('center_axis',(0.,-1.,0.));
#6834=DIRECTION('ref_axis',(1.,0.,0.));
#6835=DIRECTION('center_axis',(0.,1.,0.));
#6836=DIRECTION('ref_axis',(1.,0.,0.));
#6837=DIRECTION('',(0.,1.,0.));
#6838=DIRECTION('center_axis',(0.,1.,0.));
#6839=DIRECTION('ref_axis',(1.,0.,0.));
#6840=DIRECTION('center_axis',(0.,-1.,0.));
#6841=DIRECTION('ref_axis',(1.,0.,0.));
#6842=DIRECTION('',(-0.707106781186547,0.707106781186548,-8.65956056235493E-17));
#6843=DIRECTION('center_axis',(0.,-1.,0.));
#6844=DIRECTION('ref_axis',(0.,0.,-1.));
#6845=DIRECTION('center_axis',(0.866025403784439,0.,-0.5));
#6846=DIRECTION('ref_axis',(0.5,0.,0.866025403784439));
#6847=DIRECTION('',(-0.5,0.,-0.866025403784439));
#6848=DIRECTION('',(0.,-1.,0.));
#6849=DIRECTION('',(0.5,0.,0.866025403784439));
#6850=DIRECTION('',(0.,-1.,0.));
#6851=DIRECTION('center_axis',(1.20185167898973E-16,0.,-1.));
#6852=DIRECTION('ref_axis',(1.,0.,1.20185167898973E-16));
#6853=DIRECTION('',(-1.,0.,-1.20185167898973E-16));
#6854=DIRECTION('',(0.,-1.,0.));
#6855=DIRECTION('',(1.,0.,1.20185167898973E-16));
#6856=DIRECTION('center_axis',(-0.866025403784439,0.,-0.5));
#6857=DIRECTION('ref_axis',(0.5,0.,-0.866025403784439));
#6858=DIRECTION('',(-0.5,0.,0.866025403784439));
#6859=DIRECTION('',(0.,-1.,0.));
#6860=DIRECTION('',(0.5,0.,-0.866025403784439));
#6861=DIRECTION('center_axis',(-0.866025403784439,0.,0.5));
#6862=DIRECTION('ref_axis',(-0.5,0.,-0.866025403784439));
#6863=DIRECTION('',(0.5,0.,0.866025403784439));
#6864=DIRECTION('',(0.,-1.,0.));
#6865=DIRECTION('',(-0.5,0.,-0.866025403784439));
#6866=DIRECTION('center_axis',(-2.40370335797945E-16,0.,1.));
#6867=DIRECTION('ref_axis',(-1.,0.,-2.40370335797945E-16));
#6868=DIRECTION('',(1.,0.,2.40370335797945E-16));
#6869=DIRECTION('',(0.,-1.,0.));
#6870=DIRECTION('',(-1.,0.,-2.40370335797945E-16));
#6871=DIRECTION('center_axis',(0.866025403784439,0.,0.5));
#6872=DIRECTION('ref_axis',(-0.5,0.,0.866025403784439));
#6873=DIRECTION('',(0.5,0.,-0.866025403784439));
#6874=DIRECTION('',(-0.5,0.,0.866025403784439));
#6875=DIRECTION('center_axis',(0.,1.,0.));
#6876=DIRECTION('ref_axis',(1.,0.,0.));
#6877=DIRECTION('center_axis',(0.,-1.,0.));
#6878=DIRECTION('ref_axis',(0.,0.,-1.));
#6879=DIRECTION('',(0.,0.,1.));
#6880=DIRECTION('',(1.,0.,0.));
#6881=DIRECTION('',(0.,0.,1.));
#6882=DIRECTION('',(1.,0.,0.));
#6883=DIRECTION('',(0.,0.,1.));
#6884=DIRECTION('',(1.,0.,0.));
#6885=DIRECTION('',(0.,0.,1.));
#6886=DIRECTION('',(1.,0.,0.));
#6887=DIRECTION('',(0.,-1.,2.22044604925031E-16));
#6888=DIRECTION('',(1.,0.,0.));
#6889=DIRECTION('',(0.,-1.,2.22044604925031E-16));
#6890=DIRECTION('',(1.,0.,0.));
#6891=DIRECTION('',(0.,0.,1.));
#6892=DIRECTION('',(1.,0.,0.));
#6893=DIRECTION('',(0.,-1.,2.22044604925031E-16));
#6894=DIRECTION('',(1.,0.,0.));
#6895=DIRECTION('',(0.,-1.,2.22044604925031E-16));
#6896=DIRECTION('',(1.,0.,0.));
#6897=DIRECTION('',(0.,0.,1.));
#6898=DIRECTION('',(1.,0.,0.));
#6899=DIRECTION('',(0.,-1.,2.22044604925031E-16));
#6900=DIRECTION('',(1.,0.,0.));
#6901=DIRECTION('',(0.,-1.,2.22044604925031E-16));
#6902=DIRECTION('',(1.,0.,0.));
#6903=DIRECTION('',(0.,0.,1.));
#6904=DIRECTION('',(1.,0.,0.));
#6905=DIRECTION('',(0.,-1.,2.22044604925031E-16));
#6906=DIRECTION('',(1.,0.,0.));
#6907=DIRECTION('',(0.,-1.,2.22044604925031E-16));
#6908=DIRECTION('',(1.,0.,0.));
#6909=DIRECTION('',(0.,0.,1.));
#6910=DIRECTION('',(1.,0.,0.));
#6911=DIRECTION('',(0.,-1.,2.22044604925031E-16));
#6912=DIRECTION('',(1.,0.,0.));
#6913=DIRECTION('',(0.,-1.,2.22044604925031E-16));
#6914=DIRECTION('',(1.,0.,0.));
#6915=DIRECTION('',(0.,-1.,2.22044604925031E-16));
#6916=DIRECTION('',(1.,0.,0.));
#6917=DIRECTION('',(0.,-1.,2.22044604925031E-16));
#6918=DIRECTION('',(1.,0.,0.));
#6919=DIRECTION('',(0.,0.,1.));
#6920=DIRECTION('',(1.,0.,0.));
#6921=DIRECTION('',(0.,-1.,2.22044604925031E-16));
#6922=DIRECTION('',(1.,0.,0.));
#6923=DIRECTION('',(0.,-1.,2.22044604925031E-16));
#6924=DIRECTION('',(1.,0.,0.));
#6925=DIRECTION('',(0.,0.,1.));
#6926=DIRECTION('',(1.,0.,0.));
#6927=DIRECTION('',(0.,-1.,2.22044604925031E-16));
#6928=DIRECTION('',(1.,0.,0.));
#6929=DIRECTION('',(0.,-1.,2.22044604925031E-16));
#6930=DIRECTION('',(1.,0.,0.));
#6931=DIRECTION('',(0.,0.,1.));
#6932=DIRECTION('',(1.,0.,0.));
#6933=DIRECTION('',(0.,0.,1.));
#6934=DIRECTION('',(1.,0.,0.));
#6935=DIRECTION('',(0.,0.,1.));
#6936=DIRECTION('',(1.,0.,0.));
#6937=DIRECTION('',(0.,0.,1.));
#6938=DIRECTION('',(1.,0.,0.));
#6939=DIRECTION('',(0.,0.,1.));
#6940=DIRECTION('',(1.,0.,0.));
#6941=DIRECTION('',(0.,0.,1.));
#6942=DIRECTION('',(1.,0.,0.));
#6943=DIRECTION('axis',(0.,0.,1.));
#6944=DIRECTION('refdir',(1.,0.,0.));
#6945=DIRECTION('center_axis',(0.,1.,0.));
#6946=DIRECTION('ref_axis',(1.,0.,0.));
#6947=DIRECTION('center_axis',(0.,-1.,0.));
#6948=DIRECTION('ref_axis',(1.,0.,0.));
#6949=DIRECTION('',(0.,-1.,0.));
#6950=DIRECTION('center_axis',(0.,-1.,0.));
#6951=DIRECTION('ref_axis',(1.,0.,0.));
#6952=DIRECTION('center_axis',(0.,1.,0.));
#6953=DIRECTION('ref_axis',(1.,0.,0.));
#6954=DIRECTION('center_axis',(0.,1.,0.));
#6955=DIRECTION('ref_axis',(1.,0.,0.));
#6956=DIRECTION('',(0.,-1.,0.));
#6957=DIRECTION('center_axis',(0.,1.,0.));
#6958=DIRECTION('ref_axis',(1.,0.,0.));
#6959=DIRECTION('center_axis',(0.,1.,0.));
#6960=DIRECTION('ref_axis',(1.,0.,0.));
#6961=DIRECTION('center_axis',(0.,1.,0.));
#6962=DIRECTION('ref_axis',(1.,0.,0.));
#6963=DIRECTION('axis',(0.,0.,1.));
#6964=DIRECTION('refdir',(1.,0.,0.));
#6965=DIRECTION('center_axis',(0.,1.,0.));
#6966=DIRECTION('ref_axis',(0.,0.,1.));
#6967=DIRECTION('center_axis',(0.,-1.,0.));
#6968=DIRECTION('ref_axis',(1.,0.,0.));
#6969=DIRECTION('center_axis',(0.,-1.,0.));
#6970=DIRECTION('ref_axis',(1.,0.,0.));
#6971=DIRECTION('center_axis',(0.,-1.,0.));
#6972=DIRECTION('ref_axis',(1.,0.,0.));
#6973=DIRECTION('',(0.707106781186548,0.707106781186547,8.65956056235494E-17));
#6974=DIRECTION('center_axis',(0.,-1.,0.));
#6975=DIRECTION('ref_axis',(1.,0.,0.));
#6976=DIRECTION('center_axis',(0.,-1.,0.));
#6977=DIRECTION('ref_axis',(1.,0.,0.));
#6978=DIRECTION('',(0.,1.,0.));
#6979=DIRECTION('center_axis',(0.,1.,0.));
#6980=DIRECTION('ref_axis',(1.,0.,0.));
#6981=DIRECTION('center_axis',(0.,-1.,0.));
#6982=DIRECTION('ref_axis',(1.,0.,0.));
#6983=DIRECTION('',(-0.707106781186547,0.707106781186548,-8.65956056235493E-17));
#6984=DIRECTION('center_axis',(0.,-1.,0.));
#6985=DIRECTION('ref_axis',(0.,0.,-1.));
#6986=DIRECTION('center_axis',(0.,-1.,0.));
#6987=DIRECTION('ref_axis',(1.,0.,0.));
#6988=DIRECTION('center_axis',(0.,1.,0.));
#6989=DIRECTION('ref_axis',(1.,0.,0.));
#6990=DIRECTION('center_axis',(0.,1.,0.));
#6991=DIRECTION('ref_axis',(1.,0.,0.));
#6992=DIRECTION('',(-0.447213595499958,0.894427190999916,-5.47678698264203E-17));
#6993=DIRECTION('center_axis',(0.,-1.,0.));
#6994=DIRECTION('ref_axis',(1.,0.,0.));
#6995=DIRECTION('center_axis',(0.,1.,0.));
#6996=DIRECTION('ref_axis',(1.,0.,0.));
#6997=DIRECTION('',(0.,1.,0.));
#6998=DIRECTION('center_axis',(0.,1.,0.));
#6999=DIRECTION('ref_axis',(1.,0.,0.));
#7000=DIRECTION('center_axis',(0.,-1.,0.));
#7001=DIRECTION('ref_axis',(1.,0.,0.));
#7002=DIRECTION('',(-0.707106781186547,0.707106781186548,-8.65956056235493E-17));
#7003=DIRECTION('center_axis',(0.,-1.,0.));
#7004=DIRECTION('ref_axis',(0.,0.,-1.));
#7005=DIRECTION('center_axis',(0.866025403784439,0.,-0.5));
#7006=DIRECTION('ref_axis',(0.5,0.,0.866025403784439));
#7007=DIRECTION('',(-0.5,0.,-0.866025403784439));
#7008=DIRECTION('',(0.,-1.,0.));
#7009=DIRECTION('',(0.5,0.,0.866025403784439));
#7010=DIRECTION('',(0.,-1.,0.));
#7011=DIRECTION('center_axis',(1.92296268638356E-16,0.,-1.));
#7012=DIRECTION('ref_axis',(1.,0.,1.92296268638356E-16));
#7013=DIRECTION('',(-1.,0.,-1.92296268638356E-16));
#7014=DIRECTION('',(0.,-1.,0.));
#7015=DIRECTION('',(1.,0.,1.92296268638356E-16));
#7016=DIRECTION('center_axis',(-0.866025403784439,0.,-0.5));
#7017=DIRECTION('ref_axis',(0.5,0.,-0.866025403784439));
#7018=DIRECTION('',(-0.5,0.,0.866025403784438));
#7019=DIRECTION('',(0.,-1.,0.));
#7020=DIRECTION('',(0.5,0.,-0.866025403784438));
#7021=DIRECTION('center_axis',(-0.866025403784439,0.,0.5));
#7022=DIRECTION('ref_axis',(-0.5,0.,-0.866025403784439));
#7023=DIRECTION('',(0.5,0.,0.866025403784439));
#7024=DIRECTION('',(0.,-1.,0.));
#7025=DIRECTION('',(-0.5,0.,-0.866025403784439));
#7026=DIRECTION('center_axis',(-1.92296268638356E-16,0.,1.));
#7027=DIRECTION('ref_axis',(-1.,0.,-1.92296268638356E-16));
#7028=DIRECTION('',(1.,0.,1.92296268638356E-16));
#7029=DIRECTION('',(0.,-1.,0.));
#7030=DIRECTION('',(-1.,0.,-1.92296268638356E-16));
#7031=DIRECTION('center_axis',(0.866025403784439,0.,0.5));
#7032=DIRECTION('ref_axis',(-0.5,0.,0.866025403784439));
#7033=DIRECTION('',(0.5,0.,-0.866025403784439));
#7034=DIRECTION('',(-0.5,0.,0.866025403784439));
#7035=DIRECTION('center_axis',(0.,1.,0.));
#7036=DIRECTION('ref_axis',(1.,0.,0.));
#7037=DIRECTION('center_axis',(0.,-1.,0.));
#7038=DIRECTION('ref_axis',(0.,0.,-1.));
#7039=DIRECTION('',(0.,0.,1.));
#7040=DIRECTION('',(1.,0.,0.));
#7041=DIRECTION('',(0.,0.,1.));
#7042=DIRECTION('',(1.,0.,0.));
#7043=DIRECTION('',(0.,0.,1.));
#7044=DIRECTION('',(1.,0.,0.));
#7045=DIRECTION('',(0.,-1.,2.22044604925031E-16));
#7046=DIRECTION('',(1.,0.,0.));
#7047=DIRECTION('',(0.,-1.,2.22044604925031E-16));
#7048=DIRECTION('',(1.,0.,0.));
#7049=DIRECTION('',(0.,-1.,2.22044604925031E-16));
#7050=DIRECTION('',(1.,0.,0.));
#7051=DIRECTION('',(0.,-1.,2.22044604925031E-16));
#7052=DIRECTION('',(1.,0.,0.));
#7053=DIRECTION('',(0.,-1.,2.22044604925031E-16));
#7054=DIRECTION('',(1.,0.,0.));
#7055=DIRECTION('',(0.,-1.,2.22044604925031E-16));
#7056=DIRECTION('',(1.,0.,0.));
#7057=DIRECTION('',(0.,-1.,2.22044604925031E-16));
#7058=DIRECTION('',(1.,0.,0.));
#7059=DIRECTION('',(0.,-1.,2.22044604925031E-16));
#7060=DIRECTION('',(1.,0.,0.));
#7061=DIRECTION('',(0.,-1.,2.22044604925031E-16));
#7062=DIRECTION('',(1.,0.,0.));
#7063=DIRECTION('',(0.,-1.,2.22044604925031E-16));
#7064=DIRECTION('',(1.,0.,0.));
#7065=DIRECTION('',(0.,0.,1.));
#7066=DIRECTION('',(1.,0.,0.));
#7067=DIRECTION('',(0.,0.,1.));
#7068=DIRECTION('',(1.,0.,0.));
#7069=CARTESIAN_POINT('',(0.,0.,0.));
#7070=CARTESIAN_POINT('',(0.,0.,0.));
#7071=CARTESIAN_POINT('',(0.,0.,0.));
#7072=CARTESIAN_POINT('Origin',(2.,4.4,1.9));
#7073=CARTESIAN_POINT('',(1.835,4.4,2.));
#7074=CARTESIAN_POINT('Origin',(2.,4.4,2.));
#7075=CARTESIAN_POINT('',(1.835,4.4,2.8));
#7076=CARTESIAN_POINT('',(1.835,4.4,1.9));
#7077=CARTESIAN_POINT('Origin',(2.,4.4,2.8));
#7078=CARTESIAN_POINT('Origin',(20.,4.4,1.9));
#7079=CARTESIAN_POINT('',(19.835,4.4,2.));
#7080=CARTESIAN_POINT('Origin',(20.,4.4,2.));
#7081=CARTESIAN_POINT('',(19.835,4.4,2.8));
#7082=CARTESIAN_POINT('',(19.835,4.4,1.9));
#7083=CARTESIAN_POINT('Origin',(20.,4.4,2.8));
#7084=CARTESIAN_POINT('Origin',(23.,-2.4,1.9));
#7085=CARTESIAN_POINT('',(22.79,-2.4,2.));
#7086=CARTESIAN_POINT('Origin',(23.,-2.4,2.));
#7087=CARTESIAN_POINT('',(22.79,-2.4,2.8));
#7088=CARTESIAN_POINT('',(22.79,-2.4,1.9));
#7089=CARTESIAN_POINT('Origin',(23.,-2.4,2.8));
#7090=CARTESIAN_POINT('Origin',(-1.,2.4,1.9));
#7091=CARTESIAN_POINT('',(-1.21,2.4,2.));
#7092=CARTESIAN_POINT('Origin',(-1.,2.4,2.));
#7093=CARTESIAN_POINT('',(-1.21,2.4,2.8));
#7094=CARTESIAN_POINT('',(-1.21,2.4,1.9));
#7095=CARTESIAN_POINT('Origin',(-1.,2.4,2.8));
#7096=CARTESIAN_POINT('Origin',(-1.,-2.4,1.9));
#7097=CARTESIAN_POINT('',(-1.21,-2.4,2.));
#7098=CARTESIAN_POINT('Origin',(-1.,-2.4,2.));
#7099=CARTESIAN_POINT('',(-1.21,-2.4,2.8));
#7100=CARTESIAN_POINT('',(-1.21,-2.4,1.9));
#7101=CARTESIAN_POINT('Origin',(-1.,-2.4,2.8));
#7102=CARTESIAN_POINT('Origin',(23.,2.4,1.9));
#7103=CARTESIAN_POINT('',(22.79,2.4,2.));
#7104=CARTESIAN_POINT('Origin',(23.,2.4,2.));
#7105=CARTESIAN_POINT('',(22.79,2.4,2.8));
#7106=CARTESIAN_POINT('',(22.79,2.4,1.9));
#7107=CARTESIAN_POINT('Origin',(23.,2.4,2.8));
#7108=CARTESIAN_POINT('Origin',(19.5,-3.5,1.9));
#7109=CARTESIAN_POINT('',(19.225,-3.5,2.));
#7110=CARTESIAN_POINT('Origin',(19.5,-3.5,2.));
#7111=CARTESIAN_POINT('',(19.225,-3.5,2.8));
#7112=CARTESIAN_POINT('',(19.225,-3.5,1.9));
#7113=CARTESIAN_POINT('Origin',(19.5,-3.5,2.8));
#7114=CARTESIAN_POINT('Origin',(2.5,3.5,1.9));
#7115=CARTESIAN_POINT('',(2.225,3.5,2.));
#7116=CARTESIAN_POINT('Origin',(2.5,3.5,2.));
#7117=CARTESIAN_POINT('',(2.225,3.5,2.8));
#7118=CARTESIAN_POINT('',(2.225,3.5,1.9));
#7119=CARTESIAN_POINT('Origin',(2.5,3.5,2.8));
#7120=CARTESIAN_POINT('Origin',(2.5,-3.5,1.9));
#7121=CARTESIAN_POINT('',(2.225,-3.5,2.));
#7122=CARTESIAN_POINT('Origin',(2.5,-3.5,2.));
#7123=CARTESIAN_POINT('',(2.225,-3.5,2.8));
#7124=CARTESIAN_POINT('',(2.225,-3.5,1.9));
#7125=CARTESIAN_POINT('Origin',(2.5,-3.5,2.8));
#7126=CARTESIAN_POINT('Origin',(19.5,3.5,1.9));
#7127=CARTESIAN_POINT('',(19.225,3.5,2.));
#7128=CARTESIAN_POINT('Origin',(19.5,3.5,2.));
#7129=CARTESIAN_POINT('',(19.225,3.5,2.8));
#7130=CARTESIAN_POINT('',(19.225,3.5,1.9));
#7131=CARTESIAN_POINT('Origin',(19.5,3.5,2.8));
#7132=CARTESIAN_POINT('Origin',(14.,0.,1.9));
#7133=CARTESIAN_POINT('',(13.835,-2.02066721859312E-17,2.));
#7134=CARTESIAN_POINT('Origin',(14.,0.,2.));
#7135=CARTESIAN_POINT('',(13.835,2.02066721859312E-17,2.8));
#7136=CARTESIAN_POINT('',(13.835,-2.02066721859312E-17,1.9));
#7137=CARTESIAN_POINT('Origin',(14.,0.,2.8));
#7138=CARTESIAN_POINT('Origin',(8.,0.,1.9));
#7139=CARTESIAN_POINT('',(7.835,-2.02066721859312E-17,2.));
#7140=CARTESIAN_POINT('Origin',(8.,0.,2.));
#7141=CARTESIAN_POINT('',(7.835,2.02066721859312E-17,2.8));
#7142=CARTESIAN_POINT('',(7.835,-2.02066721859312E-17,1.9));
#7143=CARTESIAN_POINT('Origin',(8.,0.,2.8));
#7144=CARTESIAN_POINT('Origin',(2.,0.,1.9));
#7145=CARTESIAN_POINT('',(1.835,-2.02066721859313E-17,2.));
#7146=CARTESIAN_POINT('Origin',(2.,0.,2.));
#7147=CARTESIAN_POINT('',(1.835,2.02066721859313E-17,2.8));
#7148=CARTESIAN_POINT('',(1.835,-2.02066721859313E-17,1.9));
#7149=CARTESIAN_POINT('Origin',(2.,0.,2.8));
#7150=CARTESIAN_POINT('Origin',(20.,0.,1.9));
#7151=CARTESIAN_POINT('',(19.835,-2.02066721859312E-17,2.));
#7152=CARTESIAN_POINT('Origin',(20.,0.,2.));
#7153=CARTESIAN_POINT('',(19.835,2.02066721859312E-17,2.8));
#7154=CARTESIAN_POINT('',(19.835,-2.02066721859312E-17,1.9));
#7155=CARTESIAN_POINT('Origin',(20.,0.,2.8));
#7156=CARTESIAN_POINT('Origin',(24.,5.,2.));
#7157=CARTESIAN_POINT('',(24.,5.,2.));
#7158=CARTESIAN_POINT('',(-2.,5.,2.));
#7159=CARTESIAN_POINT('',(24.,5.,2.));
#7160=CARTESIAN_POINT('',(-2.,5.,2.8));
#7161=CARTESIAN_POINT('',(-2.,5.,2.));
#7162=CARTESIAN_POINT('',(24.,5.,2.8));
#7163=CARTESIAN_POINT('',(24.,5.,2.8));
#7164=CARTESIAN_POINT('',(24.,5.,2.));
#7165=CARTESIAN_POINT('Origin',(24.,-5.,2.));
#7166=CARTESIAN_POINT('',(24.,-5.,2.));
#7167=CARTESIAN_POINT('',(24.,-5.,2.));
#7168=CARTESIAN_POINT('',(24.,-5.,2.8));
#7169=CARTESIAN_POINT('',(24.,-5.,2.8));
#7170=CARTESIAN_POINT('',(24.,-5.,2.));
#7171=CARTESIAN_POINT('Origin',(-2.,-5.,2.));
#7172=CARTESIAN_POINT('',(-2.,-5.,2.));
#7173=CARTESIAN_POINT('',(-2.,-5.,2.));
#7174=CARTESIAN_POINT('',(-2.,-5.,2.8));
#7175=CARTESIAN_POINT('',(-2.,-5.,2.8));
#7176=CARTESIAN_POINT('',(-2.,-5.,2.));
#7177=CARTESIAN_POINT('Origin',(-2.,5.,2.));
#7178=CARTESIAN_POINT('',(-2.,5.,2.));
#7179=CARTESIAN_POINT('',(-2.,5.,2.8));
#7180=CARTESIAN_POINT('Origin',(11.,0.,2.8));
#7181=CARTESIAN_POINT('Origin',(11.,0.,2.));
#7182=CARTESIAN_POINT('',(0.,0.,0.));
#7183=CARTESIAN_POINT('Origin',(-0.1,0.82,-0.3));
#7184=CARTESIAN_POINT('',(0.,0.82,-0.3));
#7185=CARTESIAN_POINT('',(0.,1.,-0.3));
#7186=CARTESIAN_POINT('',(0.,0.41,-0.3));
#7187=CARTESIAN_POINT('',(30.,0.82,-0.3));
#7188=CARTESIAN_POINT('',(-0.1,0.82,-0.3));
#7189=CARTESIAN_POINT('',(30.,1.,-0.3));
#7190=CARTESIAN_POINT('',(30.,0.41,-0.3));
#7191=CARTESIAN_POINT('',(-0.05,1.,-0.3));
#7192=CARTESIAN_POINT('Origin',(-0.1,0.82,-0.55));
#7193=CARTESIAN_POINT('',(0.,0.82,-0.55));
#7194=CARTESIAN_POINT('',(0.,0.82,-0.275));
#7195=CARTESIAN_POINT('',(30.,0.82,-0.55));
#7196=CARTESIAN_POINT('',(-0.1,0.82,-0.55));
#7197=CARTESIAN_POINT('',(30.,0.82,-0.275));
#7198=CARTESIAN_POINT('Origin',(-0.1,0.67,-0.55));
#7199=CARTESIAN_POINT('',(0.,0.67,-0.55));
#7200=CARTESIAN_POINT('',(0.,0.335,-0.55));
#7201=CARTESIAN_POINT('',(30.,0.67,-0.55));
#7202=CARTESIAN_POINT('',(-0.1,0.67,-0.55));
#7203=CARTESIAN_POINT('',(30.,0.335,-0.55));
#7204=CARTESIAN_POINT('Origin',(-0.1,0.42,-0.3));
#7205=CARTESIAN_POINT('',(0.,0.42,-0.3));
#7206=CARTESIAN_POINT('',(0.,0.24,-0.12));
#7207=CARTESIAN_POINT('',(30.,0.42,-0.3));
#7208=CARTESIAN_POINT('',(-0.1,0.42,-0.3));
#7209=CARTESIAN_POINT('',(30.,0.24,-0.12));
#7210=CARTESIAN_POINT('Origin',(-0.1,0.42,0.3));
#7211=CARTESIAN_POINT('',(0.,0.42,0.3));
#7212=CARTESIAN_POINT('',(0.,0.42,0.15));
#7213=CARTESIAN_POINT('',(30.,0.42,0.3));
#7214=CARTESIAN_POINT('',(-0.1,0.42,0.3));
#7215=CARTESIAN_POINT('',(30.,0.42,0.15));
#7216=CARTESIAN_POINT('Origin',(-0.1,0.67,0.55));
#7217=CARTESIAN_POINT('',(0.,0.67,0.55));
#7218=CARTESIAN_POINT('',(6.93889390390723E-18,0.365,0.245));
#7219=CARTESIAN_POINT('',(30.,0.67,0.55));
#7220=CARTESIAN_POINT('',(-0.1,0.67,0.55));
#7221=CARTESIAN_POINT('',(30.,0.365,0.245));
#7222=CARTESIAN_POINT('Origin',(-0.1,0.82,0.55));
#7223=CARTESIAN_POINT('',(0.,0.82,0.55));
#7224=CARTESIAN_POINT('',(0.,0.41,0.55));
#7225=CARTESIAN_POINT('',(30.,0.82,0.55));
#7226=CARTESIAN_POINT('',(-0.1,0.82,0.55));
#7227=CARTESIAN_POINT('',(30.,0.41,0.55));
#7228=CARTESIAN_POINT('Origin',(-0.1,0.82,0.3));
#7229=CARTESIAN_POINT('',(0.,0.82,0.3));
#7230=CARTESIAN_POINT('',(0.,0.82,0.15));
#7231=CARTESIAN_POINT('',(30.,0.82,0.3));
#7232=CARTESIAN_POINT('',(-0.1,0.82,0.3));
#7233=CARTESIAN_POINT('',(30.,0.82,0.15));
#7234=CARTESIAN_POINT('Origin',(-0.1,1.05,0.3));
#7235=CARTESIAN_POINT('',(0.,1.,0.3));
#7236=CARTESIAN_POINT('',(0.,0.525,0.3));
#7237=CARTESIAN_POINT('',(30.,1.,0.3));
#7238=CARTESIAN_POINT('',(-0.05,1.,0.3));
#7239=CARTESIAN_POINT('',(30.,0.525,0.3));
#7240=CARTESIAN_POINT('Origin',(-0.1,-0.3,-0.82));
#7241=CARTESIAN_POINT('',(0.,-0.3,-0.82));
#7242=CARTESIAN_POINT('',(0.,-0.3,-1.));
#7243=CARTESIAN_POINT('',(0.,-0.3,-0.41));
#7244=CARTESIAN_POINT('',(30.,-0.3,-0.82));
#7245=CARTESIAN_POINT('',(-0.1,-0.3,-0.82));
#7246=CARTESIAN_POINT('',(30.,-0.3,-1.));
#7247=CARTESIAN_POINT('',(30.,-0.3,-0.41));
#7248=CARTESIAN_POINT('',(-0.05,-0.3,-1.));
#7249=CARTESIAN_POINT('Origin',(-0.1,-0.55,-0.82));
#7250=CARTESIAN_POINT('',(0.,-0.55,-0.82));
#7251=CARTESIAN_POINT('',(0.,-0.275,-0.82));
#7252=CARTESIAN_POINT('',(30.,-0.55,-0.82));
#7253=CARTESIAN_POINT('',(-0.1,-0.55,-0.82));
#7254=CARTESIAN_POINT('',(30.,-0.275,-0.82));
#7255=CARTESIAN_POINT('Origin',(-0.1,-0.55,-0.67));
#7256=CARTESIAN_POINT('',(0.,-0.55,-0.67));
#7257=CARTESIAN_POINT('',(0.,-0.55,-0.335));
#7258=CARTESIAN_POINT('',(30.,-0.55,-0.67));
#7259=CARTESIAN_POINT('',(-0.1,-0.55,-0.67));
#7260=CARTESIAN_POINT('',(30.,-0.55,-0.335));
#7261=CARTESIAN_POINT('Origin',(-0.1,-0.3,-0.42));
#7262=CARTESIAN_POINT('',(0.,-0.3,-0.42));
#7263=CARTESIAN_POINT('',(0.,-0.12,-0.24));
#7264=CARTESIAN_POINT('',(30.,-0.3,-0.42));
#7265=CARTESIAN_POINT('',(-0.1,-0.3,-0.42));
#7266=CARTESIAN_POINT('',(30.,-0.12,-0.24));
#7267=CARTESIAN_POINT('Origin',(-0.1,0.3,-0.42));
#7268=CARTESIAN_POINT('',(0.,0.3,-0.42));
#7269=CARTESIAN_POINT('',(0.,0.15,-0.42));
#7270=CARTESIAN_POINT('',(30.,0.3,-0.42));
#7271=CARTESIAN_POINT('',(-0.1,0.3,-0.42));
#7272=CARTESIAN_POINT('',(30.,0.15,-0.42));
#7273=CARTESIAN_POINT('Origin',(-0.1,0.55,-0.67));
#7274=CARTESIAN_POINT('',(0.,0.55,-0.67));
#7275=CARTESIAN_POINT('',(0.,0.245,-0.365));
#7276=CARTESIAN_POINT('',(30.,0.55,-0.67));
#7277=CARTESIAN_POINT('',(-0.1,0.55,-0.67));
#7278=CARTESIAN_POINT('',(30.,0.245,-0.365));
#7279=CARTESIAN_POINT('Origin',(-0.1,0.55,-0.82));
#7280=CARTESIAN_POINT('',(0.,0.55,-0.82));
#7281=CARTESIAN_POINT('',(0.,0.55,-0.41));
#7282=CARTESIAN_POINT('',(30.,0.55,-0.82));
#7283=CARTESIAN_POINT('',(-0.1,0.55,-0.82));
#7284=CARTESIAN_POINT('',(30.,0.55,-0.41));
#7285=CARTESIAN_POINT('Origin',(-0.1,0.3,-0.82));
#7286=CARTESIAN_POINT('',(0.,0.3,-0.82));
#7287=CARTESIAN_POINT('',(0.,0.15,-0.82));
#7288=CARTESIAN_POINT('',(30.,0.3,-0.82));
#7289=CARTESIAN_POINT('',(-0.1,0.3,-0.82));
#7290=CARTESIAN_POINT('',(30.,0.15,-0.82));
#7291=CARTESIAN_POINT('Origin',(-0.1,0.3,-1.05));
#7292=CARTESIAN_POINT('',(0.,0.3,-1.));
#7293=CARTESIAN_POINT('',(0.,0.3,-0.525));
#7294=CARTESIAN_POINT('',(30.,0.3,-1.));
#7295=CARTESIAN_POINT('',(-0.05,0.3,-1.));
#7296=CARTESIAN_POINT('',(30.,0.3,-0.525));
#7297=CARTESIAN_POINT('Origin',(-0.1,-0.82,0.3));
#7298=CARTESIAN_POINT('',(0.,-0.82,0.3));
#7299=CARTESIAN_POINT('',(0.,-1.,0.3));
#7300=CARTESIAN_POINT('',(0.,-0.41,0.3));
#7301=CARTESIAN_POINT('',(30.,-0.82,0.3));
#7302=CARTESIAN_POINT('',(-0.1,-0.82,0.3));
#7303=CARTESIAN_POINT('',(30.,-1.,0.3));
#7304=CARTESIAN_POINT('',(30.,-0.41,0.3));
#7305=CARTESIAN_POINT('',(-0.05,-1.,0.3));
#7306=CARTESIAN_POINT('Origin',(-0.1,-0.82,0.55));
#7307=CARTESIAN_POINT('',(0.,-0.82,0.55));
#7308=CARTESIAN_POINT('',(0.,-0.82,0.275));
#7309=CARTESIAN_POINT('',(30.,-0.82,0.55));
#7310=CARTESIAN_POINT('',(-0.1,-0.82,0.55));
#7311=CARTESIAN_POINT('',(30.,-0.82,0.275));
#7312=CARTESIAN_POINT('Origin',(-0.1,-0.67,0.55));
#7313=CARTESIAN_POINT('',(0.,-0.67,0.55));
#7314=CARTESIAN_POINT('',(0.,-0.335,0.55));
#7315=CARTESIAN_POINT('',(30.,-0.67,0.55));
#7316=CARTESIAN_POINT('',(-0.1,-0.67,0.55));
#7317=CARTESIAN_POINT('',(30.,-0.335,0.55));
#7318=CARTESIAN_POINT('Origin',(-0.1,-0.42,0.3));
#7319=CARTESIAN_POINT('',(0.,-0.42,0.3));
#7320=CARTESIAN_POINT('',(-6.93889390390723E-18,-0.24,0.12));
#7321=CARTESIAN_POINT('',(30.,-0.42,0.3));
#7322=CARTESIAN_POINT('',(-0.1,-0.42,0.3));
#7323=CARTESIAN_POINT('',(30.,-0.24,0.12));
#7324=CARTESIAN_POINT('Origin',(-0.1,-0.42,-0.3));
#7325=CARTESIAN_POINT('',(0.,-0.42,-0.3));
#7326=CARTESIAN_POINT('',(0.,-0.42,-0.15));
#7327=CARTESIAN_POINT('',(30.,-0.42,-0.3));
#7328=CARTESIAN_POINT('',(-0.1,-0.42,-0.3));
#7329=CARTESIAN_POINT('',(30.,-0.42,-0.15));
#7330=CARTESIAN_POINT('Origin',(-0.1,-0.67,-0.55));
#7331=CARTESIAN_POINT('',(0.,-0.67,-0.55));
#7332=CARTESIAN_POINT('',(0.,-0.365,-0.245));
#7333=CARTESIAN_POINT('',(30.,-0.67,-0.55));
#7334=CARTESIAN_POINT('',(-0.1,-0.67,-0.55));
#7335=CARTESIAN_POINT('',(30.,-0.365,-0.245));
#7336=CARTESIAN_POINT('Origin',(-0.1,-0.82,-0.55));
#7337=CARTESIAN_POINT('',(0.,-0.82,-0.55));
#7338=CARTESIAN_POINT('',(0.,-0.41,-0.55));
#7339=CARTESIAN_POINT('',(30.,-0.82,-0.55));
#7340=CARTESIAN_POINT('',(-0.1,-0.82,-0.55));
#7341=CARTESIAN_POINT('',(30.,-0.41,-0.55));
#7342=CARTESIAN_POINT('Origin',(-0.1,-0.82,-0.3));
#7343=CARTESIAN_POINT('',(0.,-0.82,-0.3));
#7344=CARTESIAN_POINT('',(0.,-0.82,-0.15));
#7345=CARTESIAN_POINT('',(30.,-0.82,-0.3));
#7346=CARTESIAN_POINT('',(-0.1,-0.82,-0.3));
#7347=CARTESIAN_POINT('',(30.,-0.82,-0.15));
#7348=CARTESIAN_POINT('Origin',(-0.1,-1.05,-0.3));
#7349=CARTESIAN_POINT('',(0.,-1.,-0.3));
#7350=CARTESIAN_POINT('',(0.,-0.525,-0.3));
#7351=CARTESIAN_POINT('',(30.,-1.,-0.3));
#7352=CARTESIAN_POINT('',(-0.05,-1.,-0.3));
#7353=CARTESIAN_POINT('',(30.,-0.525,-0.3));
#7354=CARTESIAN_POINT('Origin',(-0.1,0.3,0.82));
#7355=CARTESIAN_POINT('',(0.,0.3,0.82));
#7356=CARTESIAN_POINT('',(0.,0.3,1.));
#7357=CARTESIAN_POINT('',(0.,0.3,0.41));
#7358=CARTESIAN_POINT('',(30.,0.3,0.82));
#7359=CARTESIAN_POINT('',(-0.1,0.3,0.82));
#7360=CARTESIAN_POINT('',(30.,0.3,1.));
#7361=CARTESIAN_POINT('',(30.,0.3,0.41));
#7362=CARTESIAN_POINT('',(-0.05,0.3,1.));
#7363=CARTESIAN_POINT('Origin',(-0.1,0.55,0.82));
#7364=CARTESIAN_POINT('',(0.,0.55,0.82));
#7365=CARTESIAN_POINT('',(0.,0.275,0.82));
#7366=CARTESIAN_POINT('',(30.,0.55,0.82));
#7367=CARTESIAN_POINT('',(-0.1,0.55,0.82));
#7368=CARTESIAN_POINT('',(30.,0.275,0.82));
#7369=CARTESIAN_POINT('Origin',(-0.1,0.55,0.67));
#7370=CARTESIAN_POINT('',(0.,0.55,0.67));
#7371=CARTESIAN_POINT('',(0.,0.55,0.335));
#7372=CARTESIAN_POINT('',(30.,0.55,0.67));
#7373=CARTESIAN_POINT('',(-0.1,0.55,0.67));
#7374=CARTESIAN_POINT('',(30.,0.55,0.335));
#7375=CARTESIAN_POINT('Origin',(-0.1,0.3,0.42));
#7376=CARTESIAN_POINT('',(0.,0.3,0.42));
#7377=CARTESIAN_POINT('',(6.93889390390723E-18,0.12,0.24));
#7378=CARTESIAN_POINT('',(30.,0.3,0.42));
#7379=CARTESIAN_POINT('',(-0.1,0.3,0.42));
#7380=CARTESIAN_POINT('',(30.,0.12,0.24));
#7381=CARTESIAN_POINT('Origin',(-0.1,-0.3,0.42));
#7382=CARTESIAN_POINT('',(0.,-0.3,0.42));
#7383=CARTESIAN_POINT('',(0.,-0.15,0.42));
#7384=CARTESIAN_POINT('',(30.,-0.3,0.42));
#7385=CARTESIAN_POINT('',(-0.1,-0.3,0.42));
#7386=CARTESIAN_POINT('',(30.,-0.15,0.42));
#7387=CARTESIAN_POINT('Origin',(-0.1,-0.55,0.67));
#7388=CARTESIAN_POINT('',(0.,-0.55,0.67));
#7389=CARTESIAN_POINT('',(6.93889390390723E-18,-0.245,0.365));
#7390=CARTESIAN_POINT('',(30.,-0.55,0.67));
#7391=CARTESIAN_POINT('',(-0.1,-0.55,0.67));
#7392=CARTESIAN_POINT('',(30.,-0.245,0.365));
#7393=CARTESIAN_POINT('Origin',(-0.1,-0.55,0.82));
#7394=CARTESIAN_POINT('',(0.,-0.55,0.82));
#7395=CARTESIAN_POINT('',(0.,-0.55,0.41));
#7396=CARTESIAN_POINT('',(30.,-0.55,0.82));
#7397=CARTESIAN_POINT('',(-0.1,-0.55,0.82));
#7398=CARTESIAN_POINT('',(30.,-0.55,0.41));
#7399=CARTESIAN_POINT('Origin',(-0.1,-0.3,0.82));
#7400=CARTESIAN_POINT('',(0.,-0.3,0.82));
#7401=CARTESIAN_POINT('',(0.,-0.15,0.82));
#7402=CARTESIAN_POINT('',(30.,-0.3,0.82));
#7403=CARTESIAN_POINT('',(-0.1,-0.3,0.82));
#7404=CARTESIAN_POINT('',(30.,-0.15,0.82));
#7405=CARTESIAN_POINT('Origin',(-0.1,-0.3,1.05));
#7406=CARTESIAN_POINT('',(0.,-0.3,1.));
#7407=CARTESIAN_POINT('',(0.,-0.3,0.525));
#7408=CARTESIAN_POINT('',(30.,-0.3,1.));
#7409=CARTESIAN_POINT('',(-0.05,-0.3,1.));
#7410=CARTESIAN_POINT('',(30.,-0.3,0.525));
#7411=CARTESIAN_POINT('Origin',(-0.1,0.,0.));
#7412=CARTESIAN_POINT('',(0.,-2.57175827820944E-17,0.21));
#7413=CARTESIAN_POINT('Origin',(0.,0.,0.));
#7414=CARTESIAN_POINT('',(30.,2.57175827820944E-17,0.21));
#7415=CARTESIAN_POINT('',(-0.1,-2.57175827820944E-17,0.21));
#7416=CARTESIAN_POINT('Origin',(30.,0.,0.));
#7417=CARTESIAN_POINT('Origin',(0.,1.,-1.));
#7418=CARTESIAN_POINT('',(0.,1.,1.));
#7419=CARTESIAN_POINT('',(0.,1.,-1.));
#7420=CARTESIAN_POINT('',(30.,1.,1.));
#7421=CARTESIAN_POINT('',(0.,1.,1.));
#7422=CARTESIAN_POINT('',(30.,1.,-1.));
#7423=CARTESIAN_POINT('Origin',(0.,1.,-1.));
#7424=CARTESIAN_POINT('',(30.,1.,-1.));
#7425=CARTESIAN_POINT('',(30.,1.,-1.));
#7426=CARTESIAN_POINT('',(0.,1.,-1.));
#7427=CARTESIAN_POINT('',(0.,1.,-1.));
#7428=CARTESIAN_POINT('',(0.,1.,-1.));
#7429=CARTESIAN_POINT('Origin',(0.,-1.,-1.));
#7430=CARTESIAN_POINT('',(0.,-1.,-1.));
#7431=CARTESIAN_POINT('',(30.,-1.,-1.));
#7432=CARTESIAN_POINT('Origin',(0.,-1.,-1.));
#7433=CARTESIAN_POINT('',(30.,-1.,-1.));
#7434=CARTESIAN_POINT('',(30.,-1.,-1.));
#7435=CARTESIAN_POINT('',(0.,-1.,-1.));
#7436=CARTESIAN_POINT('',(0.,-1.,-1.));
#7437=CARTESIAN_POINT('',(0.,-1.,-1.));
#7438=CARTESIAN_POINT('Origin',(0.,-1.,1.));
#7439=CARTESIAN_POINT('',(0.,-1.,1.));
#7440=CARTESIAN_POINT('',(30.,-1.,1.));
#7441=CARTESIAN_POINT('Origin',(0.,-1.,1.));
#7442=CARTESIAN_POINT('',(30.,-1.,1.));
#7443=CARTESIAN_POINT('',(30.,-1.,1.));
#7444=CARTESIAN_POINT('',(0.,-1.,1.));
#7445=CARTESIAN_POINT('',(0.,-1.,1.));
#7446=CARTESIAN_POINT('',(0.,-1.,1.));
#7447=CARTESIAN_POINT('Origin',(0.,1.,1.));
#7448=CARTESIAN_POINT('',(0.,1.,1.));
#7449=CARTESIAN_POINT('',(30.,1.,1.));
#7450=CARTESIAN_POINT('Origin',(0.,1.,1.));
#7451=CARTESIAN_POINT('',(30.,1.,1.));
#7452=CARTESIAN_POINT('',(0.,1.,1.));
#7453=CARTESIAN_POINT('Origin',(30.,0.,0.));
#7454=CARTESIAN_POINT('Origin',(0.,0.,0.));
#7455=CARTESIAN_POINT('',(0.,0.,0.));
#7456=CARTESIAN_POINT('Origin',(0.,0.395,0.25));
#7457=CARTESIAN_POINT('',(-0.5,0.3,0.25));
#7458=CARTESIAN_POINT('',(0.5,0.3,0.25));
#7459=CARTESIAN_POINT('',(0.25,0.3,0.25));
#7460=CARTESIAN_POINT('',(-0.5,0.5,0.25));
#7461=CARTESIAN_POINT('',(-0.5,0.5,0.25));
#7462=CARTESIAN_POINT('',(0.5,0.5,0.25));
#7463=CARTESIAN_POINT('',(0.5,0.5,0.25));
#7464=CARTESIAN_POINT('',(0.5,0.29,0.25));
#7465=CARTESIAN_POINT('Origin',(0.5,0.5,0.25));
#7466=CARTESIAN_POINT('',(-0.5,0.5,0.4));
#7467=CARTESIAN_POINT('',(-0.5,0.5,0.25));
#7468=CARTESIAN_POINT('',(0.5,0.5,0.4));
#7469=CARTESIAN_POINT('',(0.5,0.5,0.4));
#7470=CARTESIAN_POINT('',(0.5,0.5,0.25));
#7471=CARTESIAN_POINT('Origin',(0.,0.,0.4));
#7472=CARTESIAN_POINT('',(-0.5,-0.5,0.4));
#7473=CARTESIAN_POINT('',(-0.5,0.5,0.4));
#7474=CARTESIAN_POINT('',(0.5,-0.5,0.4));
#7475=CARTESIAN_POINT('',(-0.5,-0.5,0.4));
#7476=CARTESIAN_POINT('',(0.5,-0.3,0.4));
#7477=CARTESIAN_POINT('',(-0.2117,2.59257727379495E-17,0.4));
#7478=CARTESIAN_POINT('Origin',(0.,0.,0.4));
#7479=CARTESIAN_POINT('Origin',(-0.5,0.3,0.));
#7480=CARTESIAN_POINT('',(-0.5,0.3,0.15));
#7481=CARTESIAN_POINT('',(-0.5,0.3,0.));
#7482=CARTESIAN_POINT('',(-0.5,0.15,0.));
#7483=CARTESIAN_POINT('',(-0.5,0.225,0.075));
#7484=CARTESIAN_POINT('',(-0.5,-0.15,0.));
#7485=CARTESIAN_POINT('',(-0.5,0.3,0.));
#7486=CARTESIAN_POINT('',(-0.5,-0.3,0.15));
#7487=CARTESIAN_POINT('',(-0.5,-0.075,-0.075));
#7488=CARTESIAN_POINT('',(-0.5,-0.3,0.25));
#7489=CARTESIAN_POINT('',(-0.5,-0.3,0.));
#7490=CARTESIAN_POINT('',(-0.5,-0.5,0.25));
#7491=CARTESIAN_POINT('',(-0.5,-0.29,0.25));
#7492=CARTESIAN_POINT('',(-0.5,-0.5,0.25));
#7493=CARTESIAN_POINT('Origin',(-0.5,-0.5,0.25));
#7494=CARTESIAN_POINT('',(0.5,-0.5,0.25));
#7495=CARTESIAN_POINT('',(-0.5,-0.5,0.25));
#7496=CARTESIAN_POINT('',(0.5,-0.5,0.25));
#7497=CARTESIAN_POINT('Origin',(0.,-0.395,0.25));
#7498=CARTESIAN_POINT('',(0.5,-0.3,0.25));
#7499=CARTESIAN_POINT('',(-0.25,-0.3,0.25));
#7500=CARTESIAN_POINT('',(0.5,-0.5,0.25));
#7501=CARTESIAN_POINT('Origin',(0.5,-0.3,0.));
#7502=CARTESIAN_POINT('',(0.5,-0.3,0.15));
#7503=CARTESIAN_POINT('',(0.5,-0.3,0.));
#7504=CARTESIAN_POINT('',(0.5,-0.15,0.));
#7505=CARTESIAN_POINT('',(0.5,-0.225,0.075));
#7506=CARTESIAN_POINT('',(0.5,0.15,0.));
#7507=CARTESIAN_POINT('',(0.5,-0.3,0.));
#7508=CARTESIAN_POINT('',(0.5,0.3,0.15));
#7509=CARTESIAN_POINT('',(0.5,0.075,-0.075));
#7510=CARTESIAN_POINT('',(0.5,0.3,0.));
#7511=CARTESIAN_POINT('Origin',(-0.5,-0.3,0.));
#7512=CARTESIAN_POINT('',(-0.25,-0.3,0.15));
#7513=CARTESIAN_POINT('Origin',(-0.25,-0.225,0.075));
#7514=CARTESIAN_POINT('',(-0.149388386429468,-0.15,0.));
#7515=CARTESIAN_POINT('',(-0.25,-0.15,0.));
#7516=CARTESIAN_POINT('',(0.149388386429468,-0.15,0.));
#7517=CARTESIAN_POINT('Origin',(0.,0.,-0.15));
#7518=CARTESIAN_POINT('',(-0.25,-0.15,0.));
#7519=CARTESIAN_POINT('Origin',(0.,0.,-0.1));
#7520=CARTESIAN_POINT('',(-0.2117,-2.59257727379495E-17,0.));
#7521=CARTESIAN_POINT('Origin',(0.,0.,0.));
#7522=CARTESIAN_POINT('',(-0.2117,-2.59257727379495E-17,-0.1));
#7523=CARTESIAN_POINT('',(-0.149388386429468,0.15,0.));
#7524=CARTESIAN_POINT('Origin',(0.,0.,0.));
#7525=CARTESIAN_POINT('',(0.149388386429468,0.15,0.));
#7526=CARTESIAN_POINT('Origin',(0.,0.,-0.15));
#7527=CARTESIAN_POINT('Origin',(0.,0.,0.));
#7528=CARTESIAN_POINT('Origin',(0.,0.,0.));
#7529=CARTESIAN_POINT('',(0.25,0.15,0.));
#7530=CARTESIAN_POINT('Origin',(0.,0.,0.));
#7531=CARTESIAN_POINT('',(0.25,0.15,0.));
#7532=CARTESIAN_POINT('Origin',(0.25,0.225,0.075));
#7533=CARTESIAN_POINT('',(0.25,0.3,0.15));
#7534=CARTESIAN_POINT('Origin',(0.5,0.3,0.));
#7535=CARTESIAN_POINT('',(0.,0.,0.));
#7536=CARTESIAN_POINT('Origin',(0.115470053837925,-0.5,-0.2));
#7537=CARTESIAN_POINT('',(0.23094010767585,-0.5,0.));
#7538=CARTESIAN_POINT('',(0.115470053837925,-0.5,-0.2));
#7539=CARTESIAN_POINT('',(0.23094010767585,-0.5,0.));
#7540=CARTESIAN_POINT('',(0.115470053837925,-0.8,-0.2));
#7541=CARTESIAN_POINT('',(0.115470053837925,-0.5,-0.2));
#7542=CARTESIAN_POINT('',(0.23094010767585,-0.8,0.));
#7543=CARTESIAN_POINT('',(0.23094010767585,-0.8,0.));
#7544=CARTESIAN_POINT('',(0.23094010767585,-0.5,0.));
#7545=CARTESIAN_POINT('Origin',(-0.115470053837925,-0.5,-0.2));
#7546=CARTESIAN_POINT('',(-0.115470053837925,-0.5,-0.2));
#7547=CARTESIAN_POINT('',(0.115470053837925,-0.5,-0.2));
#7548=CARTESIAN_POINT('',(-0.115470053837925,-0.8,-0.2));
#7549=CARTESIAN_POINT('',(-0.115470053837925,-0.5,-0.2));
#7550=CARTESIAN_POINT('',(0.115470053837925,-0.8,-0.2));
#7551=CARTESIAN_POINT('Origin',(-0.23094010767585,-0.5,-2.77555756156289E-17));
#7552=CARTESIAN_POINT('',(-0.23094010767585,-0.5,-2.82820063659975E-17));
#7553=CARTESIAN_POINT('',(-0.115470053837925,-0.5,-0.2));
#7554=CARTESIAN_POINT('',(-0.23094010767585,-0.8,-2.77555756156289E-17));
#7555=CARTESIAN_POINT('',(-0.23094010767585,-0.5,-2.82820063659975E-17));
#7556=CARTESIAN_POINT('',(-0.115470053837925,-0.8,-0.2));
#7557=CARTESIAN_POINT('Origin',(-0.115470053837925,-0.5,0.2));
#7558=CARTESIAN_POINT('',(-0.115470053837925,-0.5,0.2));
#7559=CARTESIAN_POINT('',(-0.23094010767585,-0.5,-2.82820063659975E-17));
#7560=CARTESIAN_POINT('',(-0.115470053837925,-0.8,0.2));
#7561=CARTESIAN_POINT('',(-0.115470053837925,-0.5,0.2));
#7562=CARTESIAN_POINT('',(-0.23094010767585,-0.8,-2.82820063659975E-17));
#7563=CARTESIAN_POINT('Origin',(0.115470053837925,-0.5,0.2));
#7564=CARTESIAN_POINT('',(0.115470053837925,-0.5,0.2));
#7565=CARTESIAN_POINT('',(-0.115470053837925,-0.5,0.2));
#7566=CARTESIAN_POINT('',(0.115470053837925,-0.8,0.2));
#7567=CARTESIAN_POINT('',(0.115470053837925,-0.5,0.2));
#7568=CARTESIAN_POINT('',(-0.115470053837925,-0.8,0.2));
#7569=CARTESIAN_POINT('Origin',(0.23094010767585,-0.5,0.));
#7570=CARTESIAN_POINT('',(0.115470053837925,-0.5,0.2));
#7571=CARTESIAN_POINT('',(0.115470053837925,-0.8,0.2));
#7572=CARTESIAN_POINT('Origin',(0.,-0.5,0.));
#7573=CARTESIAN_POINT('Origin',(0.,-0.8,0.));
#7574=CARTESIAN_POINT('Origin',(0.,-1.4,0.));
#7575=CARTESIAN_POINT('',(-0.24505,-1.4,3.00099698131059E-17));
#7576=CARTESIAN_POINT('Origin',(0.,-1.4,0.));
#7577=CARTESIAN_POINT('Origin',(0.375,0.5,0.));
#7578=CARTESIAN_POINT('',(-0.375,0.5,-4.59242549680257E-17));
#7579=CARTESIAN_POINT('Origin',(0.,0.5,0.));
#7580=CARTESIAN_POINT('Origin',(0.,0.475,0.));
#7581=CARTESIAN_POINT('',(-0.425,0.45,-5.20474889637625E-17));
#7582=CARTESIAN_POINT('Origin',(0.,0.45,0.));
#7583=CARTESIAN_POINT('',(-0.4,0.475,-4.89858719658941E-17));
#7584=CARTESIAN_POINT('Origin',(0.,0.24,0.));
#7585=CARTESIAN_POINT('',(-0.425,0.0299999999999998,-5.20474889637625E-17));
#7586=CARTESIAN_POINT('Origin',(0.,0.0299999999999998,0.));
#7587=CARTESIAN_POINT('',(-0.425,0.24,-5.20474889637625E-17));
#7588=CARTESIAN_POINT('Origin',(0.,0.0150000000000001,0.));
#7589=CARTESIAN_POINT('',(-0.395,4.85722573273506E-17,-4.83735485663204E-17));
#7590=CARTESIAN_POINT('Origin',(0.,0.,0.));
#7591=CARTESIAN_POINT('',(-0.41,0.0150000000000001,-5.02105187650415E-17));
#7592=CARTESIAN_POINT('Origin',(0.27,0.,0.));
#7593=CARTESIAN_POINT('',(-0.27,0.,-3.30654635769785E-17));
#7594=CARTESIAN_POINT('Origin',(0.,0.,0.));
#7595=CARTESIAN_POINT('Origin',(0.,-0.02,0.));
#7596=CARTESIAN_POINT('',(-0.24505,-0.0498999999999999,3.00099698131059E-17));
#7597=CARTESIAN_POINT('Origin',(0.,-0.0498999999999999,0.));
#7598=CARTESIAN_POINT('',(-0.26,-0.02,-3.18408167778312E-17));
#7599=CARTESIAN_POINT('Origin',(0.,-0.995,0.));
#7600=CARTESIAN_POINT('',(-0.24505,-0.995,-3.00099698131059E-17));
#7601=CARTESIAN_POINT('',(0.,0.,0.));
#7602=CARTESIAN_POINT('Origin',(14.,0.,0.97));
#7603=CARTESIAN_POINT('',(13.625,-4.59242549680257E-17,0.97));
#7604=CARTESIAN_POINT('Origin',(14.,0.,0.97));
#7605=CARTESIAN_POINT('',(13.625,4.59242549680257E-17,1.5));
#7606=CARTESIAN_POINT('',(13.625,-4.59242549680257E-17,0.97));
#7607=CARTESIAN_POINT('Origin',(14.,0.,1.5));
#7608=CARTESIAN_POINT('Origin',(14.,0.,0.97));
#7609=CARTESIAN_POINT('',(13.775,-2.75545529808154E-17,0.97));
#7610=CARTESIAN_POINT('Origin',(14.,0.,0.97));
#7611=CARTESIAN_POINT('Origin',(8.,0.,0.97));
#7612=CARTESIAN_POINT('',(7.625,-4.59242549680257E-17,0.97));
#7613=CARTESIAN_POINT('Origin',(8.,0.,0.97));
#7614=CARTESIAN_POINT('',(7.625,4.59242549680257E-17,1.5));
#7615=CARTESIAN_POINT('',(7.625,-4.59242549680257E-17,0.97));
#7616=CARTESIAN_POINT('Origin',(8.,0.,1.5));
#7617=CARTESIAN_POINT('Origin',(8.,0.,0.97));
#7618=CARTESIAN_POINT('',(7.775,-2.75545529808154E-17,0.97));
#7619=CARTESIAN_POINT('Origin',(8.,0.,0.97));
#7620=CARTESIAN_POINT('Origin',(2.,0.,0.97));
#7621=CARTESIAN_POINT('',(1.625,-4.59242549680257E-17,0.97));
#7622=CARTESIAN_POINT('Origin',(2.,0.,0.97));
#7623=CARTESIAN_POINT('',(1.625,4.59242549680257E-17,1.5));
#7624=CARTESIAN_POINT('',(1.625,-4.59242549680257E-17,0.97));
#7625=CARTESIAN_POINT('Origin',(2.,0.,1.5));
#7626=CARTESIAN_POINT('Origin',(2.,0.,0.97));
#7627=CARTESIAN_POINT('',(1.775,-2.75545529808155E-17,0.97));
#7628=CARTESIAN_POINT('Origin',(2.,0.,0.97));
#7629=CARTESIAN_POINT('Origin',(20.,0.,0.97));
#7630=CARTESIAN_POINT('',(19.625,-4.59242549680257E-17,0.97));
#7631=CARTESIAN_POINT('Origin',(20.,0.,0.97));
#7632=CARTESIAN_POINT('',(19.625,4.59242549680257E-17,1.5));
#7633=CARTESIAN_POINT('',(19.625,-4.59242549680257E-17,0.97));
#7634=CARTESIAN_POINT('Origin',(20.,0.,1.5));
#7635=CARTESIAN_POINT('Origin',(20.,0.,0.97));
#7636=CARTESIAN_POINT('',(19.775,-2.75545529808156E-17,0.97));
#7637=CARTESIAN_POINT('Origin',(20.,0.,0.97));
#7638=CARTESIAN_POINT('Origin',(14.,0.,-0.1));
#7639=CARTESIAN_POINT('',(13.775,-2.75545529808154E-17,0.));
#7640=CARTESIAN_POINT('Origin',(14.,0.,0.));
#7641=CARTESIAN_POINT('',(13.775,-2.75545529808154E-17,-0.1));
#7642=CARTESIAN_POINT('Origin',(8.,0.,-0.1));
#7643=CARTESIAN_POINT('',(7.775,-2.75545529808154E-17,0.));
#7644=CARTESIAN_POINT('Origin',(8.,0.,0.));
#7645=CARTESIAN_POINT('',(7.775,-2.75545529808154E-17,-0.1));
#7646=CARTESIAN_POINT('Origin',(2.,0.,-0.1));
#7647=CARTESIAN_POINT('',(1.775,-2.75545529808155E-17,0.));
#7648=CARTESIAN_POINT('Origin',(2.,0.,0.));
#7649=CARTESIAN_POINT('',(1.775,-2.75545529808155E-17,-0.1));
#7650=CARTESIAN_POINT('Origin',(20.,0.,-0.1));
#7651=CARTESIAN_POINT('',(19.775,-2.75545529808156E-17,0.));
#7652=CARTESIAN_POINT('Origin',(20.,0.,0.));
#7653=CARTESIAN_POINT('',(19.775,-2.75545529808156E-17,-0.1));
#7654=CARTESIAN_POINT('Origin',(0.,-0.53,1.));
#7655=CARTESIAN_POINT('',(0.,-0.53,1.));
#7656=CARTESIAN_POINT('',(0.,-0.75,0.85));
#7657=CARTESIAN_POINT('',(0.,-0.53,1.));
#7658=CARTESIAN_POINT('',(22.,-0.75,0.85));
#7659=CARTESIAN_POINT('',(0.,-0.75,0.85));
#7660=CARTESIAN_POINT('',(22.,-0.53,1.));
#7661=CARTESIAN_POINT('',(22.,-0.53,1.));
#7662=CARTESIAN_POINT('',(0.,-0.53,1.));
#7663=CARTESIAN_POINT('Origin',(0.,-0.53,1.15));
#7664=CARTESIAN_POINT('',(0.,-0.53,1.15));
#7665=CARTESIAN_POINT('',(0.,-0.53,1.15));
#7666=CARTESIAN_POINT('',(22.,-0.53,1.15));
#7667=CARTESIAN_POINT('',(22.,-0.53,1.15));
#7668=CARTESIAN_POINT('',(0.,-0.53,1.15));
#7669=CARTESIAN_POINT('Origin',(0.,-0.75,1.3));
#7670=CARTESIAN_POINT('',(0.,-0.75,1.3));
#7671=CARTESIAN_POINT('',(0.,-0.75,1.3));
#7672=CARTESIAN_POINT('',(22.,-0.75,1.3));
#7673=CARTESIAN_POINT('',(22.,-0.75,1.3));
#7674=CARTESIAN_POINT('',(0.,-0.75,1.3));
#7675=CARTESIAN_POINT('Origin',(0.,-0.75,1.5));
#7676=CARTESIAN_POINT('',(0.,-0.75,1.5));
#7677=CARTESIAN_POINT('',(0.,-0.75,1.5));
#7678=CARTESIAN_POINT('',(22.,-0.75,1.5));
#7679=CARTESIAN_POINT('',(22.,-0.75,1.5));
#7680=CARTESIAN_POINT('',(0.,-0.75,1.5));
#7681=CARTESIAN_POINT('Origin',(0.,0.75,1.5));
#7682=CARTESIAN_POINT('',(0.,0.75,1.5));
#7683=CARTESIAN_POINT('',(0.,0.75,1.5));
#7684=CARTESIAN_POINT('',(22.,0.75,1.5));
#7685=CARTESIAN_POINT('',(22.,0.75,1.5));
#7686=CARTESIAN_POINT('',(0.,0.75,1.5));
#7687=CARTESIAN_POINT('Origin',(0.,0.75,1.3));
#7688=CARTESIAN_POINT('',(0.,0.75,1.3));
#7689=CARTESIAN_POINT('',(0.,0.75,1.3));
#7690=CARTESIAN_POINT('',(22.,0.75,1.3));
#7691=CARTESIAN_POINT('',(22.,0.75,1.3));
#7692=CARTESIAN_POINT('',(0.,0.75,1.3));
#7693=CARTESIAN_POINT('Origin',(0.,0.53,1.15));
#7694=CARTESIAN_POINT('',(0.,0.53,1.15));
#7695=CARTESIAN_POINT('',(0.,0.53,1.15));
#7696=CARTESIAN_POINT('',(22.,0.53,1.15));
#7697=CARTESIAN_POINT('',(22.,0.53,1.15));
#7698=CARTESIAN_POINT('',(0.,0.53,1.15));
#7699=CARTESIAN_POINT('Origin',(0.,0.53,1.));
#7700=CARTESIAN_POINT('',(0.,0.53,1.));
#7701=CARTESIAN_POINT('',(0.,0.53,1.));
#7702=CARTESIAN_POINT('',(22.,0.53,1.));
#7703=CARTESIAN_POINT('',(22.,0.53,1.));
#7704=CARTESIAN_POINT('',(0.,0.53,1.));
#7705=CARTESIAN_POINT('Origin',(0.,0.75,0.85));
#7706=CARTESIAN_POINT('',(0.,0.75,0.85));
#7707=CARTESIAN_POINT('',(0.,0.75,0.85));
#7708=CARTESIAN_POINT('',(22.,0.75,0.85));
#7709=CARTESIAN_POINT('',(22.,0.75,0.85));
#7710=CARTESIAN_POINT('',(0.,0.75,0.85));
#7711=CARTESIAN_POINT('Origin',(0.,0.75,0.));
#7712=CARTESIAN_POINT('',(0.,0.75,0.));
#7713=CARTESIAN_POINT('',(0.,0.75,0.));
#7714=CARTESIAN_POINT('',(22.,0.75,0.));
#7715=CARTESIAN_POINT('',(22.,0.75,0.));
#7716=CARTESIAN_POINT('',(0.,0.75,0.));
#7717=CARTESIAN_POINT('Origin',(0.,-0.75,0.));
#7718=CARTESIAN_POINT('',(0.,-0.75,0.));
#7719=CARTESIAN_POINT('',(0.,-0.75,0.));
#7720=CARTESIAN_POINT('',(22.,-0.75,0.));
#7721=CARTESIAN_POINT('',(22.,-0.75,0.));
#7722=CARTESIAN_POINT('',(0.,-0.75,0.));
#7723=CARTESIAN_POINT('Origin',(0.,-0.75,0.85));
#7724=CARTESIAN_POINT('',(0.,-0.75,0.85));
#7725=CARTESIAN_POINT('',(22.,-0.75,0.85));
#7726=CARTESIAN_POINT('Origin',(22.,0.,0.75));
#7727=CARTESIAN_POINT('Origin',(0.,0.,0.75));
#7728=CARTESIAN_POINT('',(0.,0.,0.));
#7729=CARTESIAN_POINT('Origin',(0.3,0.4,0.));
#7730=CARTESIAN_POINT('',(-0.3,0.4,-3.67394039744206E-17));
#7731=CARTESIAN_POINT('Origin',(0.,0.4,0.));
#7732=CARTESIAN_POINT('Origin',(0.,0.375,0.));
#7733=CARTESIAN_POINT('',(-0.35,0.35,-4.28626379701573E-17));
#7734=CARTESIAN_POINT('Origin',(0.,0.35,0.));
#7735=CARTESIAN_POINT('',(-0.325,0.375,-3.9801020972289E-17));
#7736=CARTESIAN_POINT('Origin',(0.,0.19,0.));
#7737=CARTESIAN_POINT('',(-0.35,0.03,-4.28626379701574E-17));
#7738=CARTESIAN_POINT('Origin',(0.,0.03,0.));
#7739=CARTESIAN_POINT('',(-0.35,0.19,-4.28626379701574E-17));
#7740=CARTESIAN_POINT('Origin',(0.,0.0149999999999999,0.));
#7741=CARTESIAN_POINT('',(-0.32,-3.29597460435593E-17,-3.91886975727153E-17));
#7742=CARTESIAN_POINT('Origin',(0.,0.,0.));
#7743=CARTESIAN_POINT('',(-0.335,0.0149999999999999,-4.10256677714363E-17));
#7744=CARTESIAN_POINT('Origin',(0.22,0.,0.));
#7745=CARTESIAN_POINT('',(-0.22,-6.93889390390723E-18,-2.69422295812418E-17));
#7746=CARTESIAN_POINT('Origin',(0.,0.,0.));
#7747=CARTESIAN_POINT('Origin',(0.,-0.02,0.));
#7748=CARTESIAN_POINT('',(-0.1954,-0.0492,2.39295984553393E-17));
#7749=CARTESIAN_POINT('Origin',(0.,-0.0492,0.));
#7750=CARTESIAN_POINT('',(-0.21,-0.02,-2.57175827820944E-17));
#7751=CARTESIAN_POINT('Origin',(0.,-0.8,0.));
#7752=CARTESIAN_POINT('',(-0.1954,-1.5646,2.39295984553393E-17));
#7753=CARTESIAN_POINT('Origin',(0.,-1.5646,0.));
#7754=CARTESIAN_POINT('',(-0.1954,-0.8,-2.39295984553393E-17));
#7755=CARTESIAN_POINT('Origin',(0.,-1.58,0.));
#7756=CARTESIAN_POINT('',(-0.16,-1.6,-1.95943487863577E-17));
#7757=CARTESIAN_POINT('Origin',(0.,-1.6,0.));
#7758=CARTESIAN_POINT('',(-0.18,-1.58,-2.20436423846524E-17));
#7759=CARTESIAN_POINT('Origin',(0.,-1.6,0.));
#7760=CARTESIAN_POINT('Origin',(0.0866025403784439,-0.4,-0.15));
#7761=CARTESIAN_POINT('',(0.173205080756888,-0.4,0.));
#7762=CARTESIAN_POINT('',(0.0866025403784439,-0.4,-0.15));
#7763=CARTESIAN_POINT('',(0.173205080756888,-0.4,0.));
#7764=CARTESIAN_POINT('',(0.0866025403784439,-0.64,-0.15));
#7765=CARTESIAN_POINT('',(0.0866025403784439,-0.4,-0.15));
#7766=CARTESIAN_POINT('',(0.173205080756888,-0.64,0.));
#7767=CARTESIAN_POINT('',(0.173205080756888,-0.64,0.));
#7768=CARTESIAN_POINT('',(0.173205080756888,-0.4,0.));
#7769=CARTESIAN_POINT('Origin',(-0.0866025403784438,-0.4,-0.15));
#7770=CARTESIAN_POINT('',(-0.0866025403784438,-0.4,-0.15));
#7771=CARTESIAN_POINT('',(0.0866025403784439,-0.4,-0.15));
#7772=CARTESIAN_POINT('',(-0.0866025403784438,-0.64,-0.15));
#7773=CARTESIAN_POINT('',(-0.0866025403784438,-0.4,-0.15));
#7774=CARTESIAN_POINT('',(0.0866025403784439,-0.64,-0.15));
#7775=CARTESIAN_POINT('Origin',(-0.173205080756888,-0.4,-2.77555756156289E-17));
#7776=CARTESIAN_POINT('',(-0.173205080756888,-0.4,-2.12115047744981E-17));
#7777=CARTESIAN_POINT('',(-0.0866025403784438,-0.4,-0.15));
#7778=CARTESIAN_POINT('',(-0.173205080756888,-0.64,-2.77555756156289E-17));
#7779=CARTESIAN_POINT('',(-0.173205080756888,-0.4,-2.12115047744981E-17));
#7780=CARTESIAN_POINT('',(-0.0866025403784438,-0.64,-0.15));
#7781=CARTESIAN_POINT('Origin',(-0.0866025403784439,-0.4,0.15));
#7782=CARTESIAN_POINT('',(-0.0866025403784439,-0.4,0.15));
#7783=CARTESIAN_POINT('',(-0.173205080756888,-0.4,-2.12115047744981E-17));
#7784=CARTESIAN_POINT('',(-0.0866025403784439,-0.64,0.15));
#7785=CARTESIAN_POINT('',(-0.0866025403784439,-0.4,0.15));
#7786=CARTESIAN_POINT('',(-0.173205080756888,-0.64,-2.12115047744981E-17));
#7787=CARTESIAN_POINT('Origin',(0.0866025403784439,-0.4,0.15));
#7788=CARTESIAN_POINT('',(0.0866025403784439,-0.4,0.15));
#7789=CARTESIAN_POINT('',(-0.0866025403784439,-0.4,0.15));
#7790=CARTESIAN_POINT('',(0.0866025403784439,-0.64,0.15));
#7791=CARTESIAN_POINT('',(0.0866025403784439,-0.4,0.15));
#7792=CARTESIAN_POINT('',(-0.0866025403784439,-0.64,0.15));
#7793=CARTESIAN_POINT('Origin',(0.173205080756888,-0.4,0.));
#7794=CARTESIAN_POINT('',(0.0866025403784439,-0.4,0.15));
#7795=CARTESIAN_POINT('',(0.0866025403784439,-0.64,0.15));
#7796=CARTESIAN_POINT('Origin',(0.,-0.4,-2.77555756156289E-17));
#7797=CARTESIAN_POINT('Origin',(0.,-0.64,-2.77555756156289E-17));
#7798=CARTESIAN_POINT('',(0.,0.,0.));
#7799=CARTESIAN_POINT('Origin',(-1.,-2.4,4.));
#7800=CARTESIAN_POINT('',(-1.475,-2.4,4.));
#7801=CARTESIAN_POINT('Origin',(-1.,-2.4,4.));
#7802=CARTESIAN_POINT('',(-1.475,-2.4,6.2));
#7803=CARTESIAN_POINT('',(-1.475,-2.4,4.));
#7804=CARTESIAN_POINT('Origin',(-1.,-2.4,6.2));
#7805=CARTESIAN_POINT('Origin',(-1.,-2.4,4.));
#7806=CARTESIAN_POINT('',(-1.275,-2.4,4.));
#7807=CARTESIAN_POINT('Origin',(-1.,-2.4,4.));
#7808=CARTESIAN_POINT('Origin',(-1.,2.4,4.));
#7809=CARTESIAN_POINT('',(-1.475,2.4,4.));
#7810=CARTESIAN_POINT('Origin',(-1.,2.4,4.));
#7811=CARTESIAN_POINT('',(-1.475,2.4,6.2));
#7812=CARTESIAN_POINT('',(-1.475,2.4,4.));
#7813=CARTESIAN_POINT('Origin',(-1.,2.4,6.2));
#7814=CARTESIAN_POINT('Origin',(-1.,2.4,4.));
#7815=CARTESIAN_POINT('',(-1.275,2.4,4.));
#7816=CARTESIAN_POINT('Origin',(-1.,2.4,4.));
#7817=CARTESIAN_POINT('Origin',(-1.,-2.4,2.7));
#7818=CARTESIAN_POINT('',(-1.275,-2.4,2.8));
#7819=CARTESIAN_POINT('Origin',(-1.,-2.4,2.8));
#7820=CARTESIAN_POINT('',(-1.275,-2.4,2.7));
#7821=CARTESIAN_POINT('Origin',(-1.,2.4,2.7));
#7822=CARTESIAN_POINT('',(-1.275,2.4,2.8));
#7823=CARTESIAN_POINT('Origin',(-1.,2.4,2.8));
#7824=CARTESIAN_POINT('',(-1.275,2.4,2.7));
#7825=CARTESIAN_POINT('Origin',(0.,3.2,2.8));
#7826=CARTESIAN_POINT('',(0.,3.2,2.8));
#7827=CARTESIAN_POINT('',(-2.,3.2,2.8));
#7828=CARTESIAN_POINT('',(0.,3.2,2.8));
#7829=CARTESIAN_POINT('',(-2.,3.2,6.2));
#7830=CARTESIAN_POINT('',(-2.,3.2,2.8));
#7831=CARTESIAN_POINT('',(0.,3.2,6.2));
#7832=CARTESIAN_POINT('',(0.,3.2,6.2));
#7833=CARTESIAN_POINT('',(0.,3.2,2.8));
#7834=CARTESIAN_POINT('Origin',(0.,-3.2,2.8));
#7835=CARTESIAN_POINT('',(0.,-3.2,2.8));
#7836=CARTESIAN_POINT('',(0.,-3.2,2.8));
#7837=CARTESIAN_POINT('',(0.,-3.2,6.2));
#7838=CARTESIAN_POINT('',(0.,-3.2,6.2));
#7839=CARTESIAN_POINT('',(0.,-3.2,2.8));
#7840=CARTESIAN_POINT('Origin',(-2.,-3.2,2.8));
#7841=CARTESIAN_POINT('',(-2.,-3.2,2.8));
#7842=CARTESIAN_POINT('',(-2.,-3.2,2.8));
#7843=CARTESIAN_POINT('',(-2.,-3.2,6.2));
#7844=CARTESIAN_POINT('',(-2.,-3.2,6.2));
#7845=CARTESIAN_POINT('',(-2.,-3.2,2.8));
#7846=CARTESIAN_POINT('Origin',(-2.,3.2,2.8));
#7847=CARTESIAN_POINT('',(-2.,3.2,2.8));
#7848=CARTESIAN_POINT('',(-2.,3.2,6.2));
#7849=CARTESIAN_POINT('Origin',(-1.,0.,6.2));
#7850=CARTESIAN_POINT('Origin',(-1.,0.,2.8));
#7851=CARTESIAN_POINT('',(0.,0.,0.));
#7852=CARTESIAN_POINT('Origin',(0.2,3.,5.2));
#7853=CARTESIAN_POINT('',(0.2,3.,5.2));
#7854=CARTESIAN_POINT('',(0.,3.,5.2));
#7855=CARTESIAN_POINT('',(0.2,3.,5.2));
#7856=CARTESIAN_POINT('',(0.,3.,6.2));
#7857=CARTESIAN_POINT('',(0.,3.,5.2));
#7858=CARTESIAN_POINT('',(0.2,3.,6.2));
#7859=CARTESIAN_POINT('',(0.2,3.,6.2));
#7860=CARTESIAN_POINT('',(0.2,3.,5.2));
#7861=CARTESIAN_POINT('Origin',(0.2,-3.,5.2));
#7862=CARTESIAN_POINT('',(0.2,-3.,5.2));
#7863=CARTESIAN_POINT('',(0.2,-3.,5.2));
#7864=CARTESIAN_POINT('',(0.2,-3.,6.2));
#7865=CARTESIAN_POINT('',(0.2,-3.,6.2));
#7866=CARTESIAN_POINT('',(0.2,-3.,5.2));
#7867=CARTESIAN_POINT('Origin',(0.,-3.,5.2));
#7868=CARTESIAN_POINT('',(0.,-3.,5.2));
#7869=CARTESIAN_POINT('',(0.,-3.,5.2));
#7870=CARTESIAN_POINT('',(0.,-3.,6.2));
#7871=CARTESIAN_POINT('',(0.,-3.,6.2));
#7872=CARTESIAN_POINT('',(0.,-3.,5.2));
#7873=CARTESIAN_POINT('Origin',(0.,3.,5.2));
#7874=CARTESIAN_POINT('',(0.,3.,5.2));
#7875=CARTESIAN_POINT('',(0.,3.,6.2));
#7876=CARTESIAN_POINT('Origin',(0.1,0.,6.2));
#7877=CARTESIAN_POINT('Origin',(0.1,0.,5.2));
#7878=CARTESIAN_POINT('',(0.,0.,0.));
#7879=CARTESIAN_POINT('Origin',(4.,-2.5,-0.3));
#7880=CARTESIAN_POINT('',(4.,-2.5,-0.3));
#7881=CARTESIAN_POINT('',(2.,-2.5,-0.3));
#7882=CARTESIAN_POINT('',(4.,-2.5,-0.3));
#7883=CARTESIAN_POINT('',(2.,-2.5,0.));
#7884=CARTESIAN_POINT('',(2.,-2.5,-0.3));
#7885=CARTESIAN_POINT('',(4.,-2.5,0.));
#7886=CARTESIAN_POINT('',(4.,-2.5,0.));
#7887=CARTESIAN_POINT('',(4.,-2.5,-0.3));
#7888=CARTESIAN_POINT('Origin',(4.,-4.5,-0.3));
#7889=CARTESIAN_POINT('',(4.,-4.5,-0.3));
#7890=CARTESIAN_POINT('',(4.,-4.5,-0.3));
#7891=CARTESIAN_POINT('',(4.,-4.5,0.));
#7892=CARTESIAN_POINT('',(4.,-4.5,0.));
#7893=CARTESIAN_POINT('',(4.,-4.5,-0.3));
#7894=CARTESIAN_POINT('Origin',(2.,-4.5,-0.3));
#7895=CARTESIAN_POINT('',(2.,-4.5,-0.3));
#7896=CARTESIAN_POINT('',(2.,-4.5,-0.3));
#7897=CARTESIAN_POINT('',(2.,-4.5,0.));
#7898=CARTESIAN_POINT('',(2.,-4.5,0.));
#7899=CARTESIAN_POINT('',(2.,-4.5,-0.3));
#7900=CARTESIAN_POINT('Origin',(2.,-2.5,-0.3));
#7901=CARTESIAN_POINT('',(2.,-2.5,-0.3));
#7902=CARTESIAN_POINT('',(2.,-2.5,0.));
#7903=CARTESIAN_POINT('Origin',(3.,-3.5,0.));
#7904=CARTESIAN_POINT('Origin',(3.,-3.5,-0.3));
#7905=CARTESIAN_POINT('',(0.,0.,0.));
#7906=CARTESIAN_POINT('',(0.,0.,0.));
#7907=CARTESIAN_POINT('',(0.,0.,0.));
#7908=CARTESIAN_POINT('Origin',(1.5,-1.9,1.7));
#7909=CARTESIAN_POINT('',(1.56403124237433,-1.7,1.7));
#7910=CARTESIAN_POINT('',(1.43596875762567,-1.7,1.7));
#7911=CARTESIAN_POINT('',(0.75,-1.7,1.7));
#7912=CARTESIAN_POINT('Origin',(1.5,-1.9,1.7));
#7913=CARTESIAN_POINT('Origin',(1.5,-1.9,1.7));
#7914=CARTESIAN_POINT('',(1.56403124237433,-1.7,1.75));
#7915=CARTESIAN_POINT('',(1.56403124237433,-1.7,1.7));
#7916=CARTESIAN_POINT('',(1.29,-1.9,1.75));
#7917=CARTESIAN_POINT('Origin',(1.5,-1.9,1.75));
#7918=CARTESIAN_POINT('',(1.29,-1.9,2.4));
#7919=CARTESIAN_POINT('',(1.29,-1.9,1.7));
#7920=CARTESIAN_POINT('Origin',(1.5,-1.9,2.4));
#7921=CARTESIAN_POINT('',(1.43596875762567,-1.7,1.75));
#7922=CARTESIAN_POINT('Origin',(1.5,-1.9,1.75));
#7923=CARTESIAN_POINT('',(1.43596875762567,-1.7,1.7));
#7924=CARTESIAN_POINT('Origin',(-1.5,1.9,1.7));
#7925=CARTESIAN_POINT('',(-1.56403124237433,1.7,1.7));
#7926=CARTESIAN_POINT('',(-1.43596875762567,1.7,1.7));
#7927=CARTESIAN_POINT('',(-0.75,1.7,1.7));
#7928=CARTESIAN_POINT('Origin',(-1.5,1.9,1.7));
#7929=CARTESIAN_POINT('Origin',(-1.5,1.9,1.7));
#7930=CARTESIAN_POINT('',(-1.56403124237433,1.7,1.75));
#7931=CARTESIAN_POINT('',(-1.56403124237433,1.7,1.7));
#7932=CARTESIAN_POINT('',(-1.71,1.9,1.75));
#7933=CARTESIAN_POINT('Origin',(-1.5,1.9,1.75));
#7934=CARTESIAN_POINT('',(-1.71,1.9,2.4));
#7935=CARTESIAN_POINT('',(-1.71,1.9,1.7));
#7936=CARTESIAN_POINT('Origin',(-1.5,1.9,2.4));
#7937=CARTESIAN_POINT('',(-1.43596875762567,1.7,1.75));
#7938=CARTESIAN_POINT('Origin',(-1.5,1.9,1.75));
#7939=CARTESIAN_POINT('',(-1.43596875762567,1.7,1.7));
#7940=CARTESIAN_POINT('Origin',(-1.5,-1.9,1.7));
#7941=CARTESIAN_POINT('',(-1.43596875762567,-1.7,1.7));
#7942=CARTESIAN_POINT('',(-1.56403124237433,-1.7,1.7));
#7943=CARTESIAN_POINT('',(-0.75,-1.7,1.7));
#7944=CARTESIAN_POINT('Origin',(-1.5,-1.9,1.7));
#7945=CARTESIAN_POINT('Origin',(-1.5,-1.9,1.7));
#7946=CARTESIAN_POINT('',(-1.43596875762567,-1.7,1.75));
#7947=CARTESIAN_POINT('',(-1.43596875762567,-1.7,1.7));
#7948=CARTESIAN_POINT('',(-1.71,-1.9,1.75));
#7949=CARTESIAN_POINT('Origin',(-1.5,-1.9,1.75));
#7950=CARTESIAN_POINT('',(-1.71,-1.9,2.4));
#7951=CARTESIAN_POINT('',(-1.71,-1.9,1.7));
#7952=CARTESIAN_POINT('Origin',(-1.5,-1.9,2.4));
#7953=CARTESIAN_POINT('',(-1.56403124237433,-1.7,1.75));
#7954=CARTESIAN_POINT('Origin',(-1.5,-1.9,1.75));
#7955=CARTESIAN_POINT('',(-1.56403124237433,-1.7,1.7));
#7956=CARTESIAN_POINT('Origin',(1.5,1.9,1.7));
#7957=CARTESIAN_POINT('',(1.43596875762567,1.7,1.7));
#7958=CARTESIAN_POINT('',(1.56403124237433,1.7,1.7));
#7959=CARTESIAN_POINT('',(0.75,1.7,1.7));
#7960=CARTESIAN_POINT('Origin',(1.5,1.9,1.7));
#7961=CARTESIAN_POINT('Origin',(1.5,1.9,1.7));
#7962=CARTESIAN_POINT('',(1.43596875762567,1.7,1.75));
#7963=CARTESIAN_POINT('',(1.43596875762567,1.7,1.7));
#7964=CARTESIAN_POINT('',(1.29,1.9,1.75));
#7965=CARTESIAN_POINT('Origin',(1.5,1.9,1.75));
#7966=CARTESIAN_POINT('',(1.29,1.9,2.4));
#7967=CARTESIAN_POINT('',(1.29,1.9,1.7));
#7968=CARTESIAN_POINT('Origin',(1.5,1.9,2.4));
#7969=CARTESIAN_POINT('',(1.56403124237433,1.7,1.75));
#7970=CARTESIAN_POINT('Origin',(1.5,1.9,1.75));
#7971=CARTESIAN_POINT('',(1.56403124237433,1.7,1.7));
#7972=CARTESIAN_POINT('Origin',(0.,-1.7,1.75));
#7973=CARTESIAN_POINT('',(0.,-1.7,1.75));
#7974=CARTESIAN_POINT('',(-1.97,-1.7,1.75));
#7975=CARTESIAN_POINT('',(0.,-1.7,1.75));
#7976=CARTESIAN_POINT('',(-1.97,-1.7,0.43));
#7977=CARTESIAN_POINT('',(-1.97,-1.7,1.75));
#7978=CARTESIAN_POINT('',(1.97,-1.7,0.43));
#7979=CARTESIAN_POINT('',(0.,-1.7,0.43));
#7980=CARTESIAN_POINT('',(1.97,-1.7,1.75));
#7981=CARTESIAN_POINT('',(1.97,-1.7,1.75));
#7982=CARTESIAN_POINT('',(0.,-1.7,1.75));
#7983=CARTESIAN_POINT('Origin',(0.,1.7,0.43));
#7984=CARTESIAN_POINT('',(0.,1.7,1.75));
#7985=CARTESIAN_POINT('',(1.97,1.7,1.75));
#7986=CARTESIAN_POINT('',(0.,1.7,1.75));
#7987=CARTESIAN_POINT('',(1.97,1.7,0.43));
#7988=CARTESIAN_POINT('',(1.97,1.7,0.43));
#7989=CARTESIAN_POINT('',(-1.97,1.7,0.43));
#7990=CARTESIAN_POINT('',(0.,1.7,0.43));
#7991=CARTESIAN_POINT('',(-1.97,1.7,1.75));
#7992=CARTESIAN_POINT('',(-1.97,1.7,0.43));
#7993=CARTESIAN_POINT('',(0.,1.7,1.75));
#7994=CARTESIAN_POINT('Origin',(-1.97,0.,1.415));
#7995=CARTESIAN_POINT('',(-1.97,-2.35,1.75));
#7996=CARTESIAN_POINT('',(-1.97,-2.35,1.75));
#7997=CARTESIAN_POINT('',(-1.97,-2.35,2.4));
#7998=CARTESIAN_POINT('',(-1.97,-2.35,2.4));
#7999=CARTESIAN_POINT('',(-1.97,2.35,2.4));
#8000=CARTESIAN_POINT('',(-1.97,2.35,2.4));
#8001=CARTESIAN_POINT('',(-1.97,2.35,1.75));
#8002=CARTESIAN_POINT('',(-1.97,2.35,1.75));
#8003=CARTESIAN_POINT('',(-1.97,1.7,1.75));
#8004=CARTESIAN_POINT('',(-1.97,0.78,0.43));
#8005=CARTESIAN_POINT('',(-1.97,0.78,0.43));
#8006=CARTESIAN_POINT('',(-1.97,0.78,1.55));
#8007=CARTESIAN_POINT('',(-1.97,0.78,1.55));
#8008=CARTESIAN_POINT('',(-1.97,-0.78,1.55));
#8009=CARTESIAN_POINT('',(-1.97,-0.78,1.55));
#8010=CARTESIAN_POINT('',(-1.97,-0.78,0.43));
#8011=CARTESIAN_POINT('',(-1.97,-0.78,0.43));
#8012=CARTESIAN_POINT('',(-1.97,-1.7,0.43));
#8013=CARTESIAN_POINT('Origin',(0.,-2.35,1.75));
#8014=CARTESIAN_POINT('',(1.97,-2.35,1.75));
#8015=CARTESIAN_POINT('',(1.97,-2.35,1.75));
#8016=CARTESIAN_POINT('',(0.,-2.35,1.75));
#8017=CARTESIAN_POINT('Origin',(0.,-2.35,2.4));
#8018=CARTESIAN_POINT('',(1.97,-2.35,2.4));
#8019=CARTESIAN_POINT('',(1.97,-2.35,2.4));
#8020=CARTESIAN_POINT('',(0.,-2.35,2.4));
#8021=CARTESIAN_POINT('Origin',(0.,2.35,2.4));
#8022=CARTESIAN_POINT('',(1.97,2.35,2.4));
#8023=CARTESIAN_POINT('',(1.97,2.35,2.4));
#8024=CARTESIAN_POINT('',(0.,2.35,2.4));
#8025=CARTESIAN_POINT('Origin',(0.,2.35,1.75));
#8026=CARTESIAN_POINT('',(1.97,2.35,1.75));
#8027=CARTESIAN_POINT('',(1.97,2.35,1.75));
#8028=CARTESIAN_POINT('',(0.,2.35,1.75));
#8029=CARTESIAN_POINT('Origin',(0.,1.7,1.75));
#8030=CARTESIAN_POINT('',(1.97,1.7,1.75));
#8031=CARTESIAN_POINT('Origin',(0.,0.78,0.43));
#8032=CARTESIAN_POINT('',(1.97,0.78,0.43));
#8033=CARTESIAN_POINT('',(1.97,0.78,0.43));
#8034=CARTESIAN_POINT('',(0.,0.78,0.43));
#8035=CARTESIAN_POINT('Origin',(0.,0.78,1.55));
#8036=CARTESIAN_POINT('',(1.97,0.78,1.55));
#8037=CARTESIAN_POINT('',(1.97,0.78,1.55));
#8038=CARTESIAN_POINT('',(0.,0.78,1.55));
#8039=CARTESIAN_POINT('Origin',(0.,-0.78,1.55));
#8040=CARTESIAN_POINT('',(1.97,-0.78,1.55));
#8041=CARTESIAN_POINT('',(1.97,-0.78,1.55));
#8042=CARTESIAN_POINT('',(0.,-0.78,1.55));
#8043=CARTESIAN_POINT('Origin',(0.,-0.78,0.43));
#8044=CARTESIAN_POINT('',(1.97,-0.78,0.43));
#8045=CARTESIAN_POINT('',(1.97,-0.78,0.43));
#8046=CARTESIAN_POINT('',(0.,-0.78,0.43));
#8047=CARTESIAN_POINT('Origin',(0.,-1.7,0.43));
#8048=CARTESIAN_POINT('',(1.97,-1.7,0.43));
#8049=CARTESIAN_POINT('Origin',(1.97,0.,1.415));
#8050=CARTESIAN_POINT('',(0.,0.,0.));
#8051=CARTESIAN_POINT('Origin',(1.97,1.7,2.3));
#8052=CARTESIAN_POINT('',(1.97,1.7,2.3));
#8053=CARTESIAN_POINT('',(1.97,-1.7,2.3));
#8054=CARTESIAN_POINT('',(1.97,1.7,2.3));
#8055=CARTESIAN_POINT('',(3.07,-1.7,2.3));
#8056=CARTESIAN_POINT('',(1.97,-1.7,2.3));
#8057=CARTESIAN_POINT('',(3.07,1.7,2.3));
#8058=CARTESIAN_POINT('',(3.07,1.7,2.3));
#8059=CARTESIAN_POINT('',(1.97,1.7,2.3));
#8060=CARTESIAN_POINT('Origin',(1.97,1.7,0.46));
#8061=CARTESIAN_POINT('',(1.97,1.7,0.46));
#8062=CARTESIAN_POINT('',(1.97,1.7,0.46));
#8063=CARTESIAN_POINT('',(3.07,1.7,0.46));
#8064=CARTESIAN_POINT('',(3.07,1.7,0.46));
#8065=CARTESIAN_POINT('',(1.97,1.7,0.46));
#8066=CARTESIAN_POINT('Origin',(1.97,0.78,0.46));
#8067=CARTESIAN_POINT('',(1.97,0.78,0.46));
#8068=CARTESIAN_POINT('',(1.97,0.78,0.46));
#8069=CARTESIAN_POINT('',(3.07,0.78,0.46));
#8070=CARTESIAN_POINT('',(3.07,0.78,0.46));
#8071=CARTESIAN_POINT('',(1.97,0.78,0.46));
#8072=CARTESIAN_POINT('Origin',(1.97,0.78,1.55));
#8073=CARTESIAN_POINT('',(1.97,0.78,1.55));
#8074=CARTESIAN_POINT('',(1.97,0.78,1.55));
#8075=CARTESIAN_POINT('',(3.07,0.78,1.55));
#8076=CARTESIAN_POINT('',(3.07,0.78,1.55));
#8077=CARTESIAN_POINT('',(1.97,0.78,1.55));
#8078=CARTESIAN_POINT('Origin',(1.97,-0.78,1.55));
#8079=CARTESIAN_POINT('',(1.97,-0.78,1.55));
#8080=CARTESIAN_POINT('',(1.97,-0.78,1.55));
#8081=CARTESIAN_POINT('',(3.07,-0.78,1.55));
#8082=CARTESIAN_POINT('',(3.07,-0.78,1.55));
#8083=CARTESIAN_POINT('',(1.97,-0.78,1.55));
#8084=CARTESIAN_POINT('Origin',(1.97,-0.78,0.46));
#8085=CARTESIAN_POINT('',(1.97,-0.78,0.46));
#8086=CARTESIAN_POINT('',(1.97,-0.78,0.46));
#8087=CARTESIAN_POINT('',(3.07,-0.78,0.46));
#8088=CARTESIAN_POINT('',(3.07,-0.78,0.46));
#8089=CARTESIAN_POINT('',(1.97,-0.78,0.46));
#8090=CARTESIAN_POINT('Origin',(1.97,-1.7,0.46));
#8091=CARTESIAN_POINT('',(1.97,-1.7,0.46));
#8092=CARTESIAN_POINT('',(1.97,-1.7,0.46));
#8093=CARTESIAN_POINT('',(3.07,-1.7,0.46));
#8094=CARTESIAN_POINT('',(3.07,-1.7,0.46));
#8095=CARTESIAN_POINT('',(1.97,-1.7,0.46));
#8096=CARTESIAN_POINT('Origin',(1.97,-1.7,2.3));
#8097=CARTESIAN_POINT('',(1.97,-1.7,2.3));
#8098=CARTESIAN_POINT('',(3.07,-1.7,2.3));
#8099=CARTESIAN_POINT('Origin',(3.07,0.,1.38));
#8100=CARTESIAN_POINT('Origin',(1.97,0.,1.38));
#8101=CARTESIAN_POINT('',(0.,0.,0.));
#8102=CARTESIAN_POINT('Origin',(-1.97,-0.78,0.46));
#8103=CARTESIAN_POINT('',(-1.97,-1.7,0.46));
#8104=CARTESIAN_POINT('',(-1.97,-0.78,0.46));
#8105=CARTESIAN_POINT('',(-1.97,-1.7,0.46));
#8106=CARTESIAN_POINT('',(-3.07,-1.7,0.46));
#8107=CARTESIAN_POINT('',(-1.97,-1.7,0.46));
#8108=CARTESIAN_POINT('',(-3.07,-0.78,0.46));
#8109=CARTESIAN_POINT('',(-3.07,-1.7,0.46));
#8110=CARTESIAN_POINT('',(-1.97,-0.78,0.46));
#8111=CARTESIAN_POINT('Origin',(-1.97,-0.78,1.55));
#8112=CARTESIAN_POINT('',(-1.97,-0.78,1.55));
#8113=CARTESIAN_POINT('',(-1.97,-0.78,0.46));
#8114=CARTESIAN_POINT('',(-3.07,-0.78,1.55));
#8115=CARTESIAN_POINT('',(-3.07,-0.78,0.46));
#8116=CARTESIAN_POINT('',(-1.97,-0.78,1.55));
#8117=CARTESIAN_POINT('Origin',(-1.97,0.78,1.55));
#8118=CARTESIAN_POINT('',(-1.97,0.78,1.55));
#8119=CARTESIAN_POINT('',(-1.97,-0.78,1.55));
#8120=CARTESIAN_POINT('',(-3.07,0.78,1.55));
#8121=CARTESIAN_POINT('',(-3.07,-0.78,1.55));
#8122=CARTESIAN_POINT('',(-1.97,0.78,1.55));
#8123=CARTESIAN_POINT('Origin',(-1.97,0.78,0.46));
#8124=CARTESIAN_POINT('',(-1.97,0.78,0.46));
#8125=CARTESIAN_POINT('',(-1.97,0.78,1.55));
#8126=CARTESIAN_POINT('',(-3.07,0.78,0.46));
#8127=CARTESIAN_POINT('',(-3.07,0.78,1.55));
#8128=CARTESIAN_POINT('',(-1.97,0.78,0.46));
#8129=CARTESIAN_POINT('Origin',(-1.97,1.7,0.46));
#8130=CARTESIAN_POINT('',(-1.97,1.7,0.46));
#8131=CARTESIAN_POINT('',(-1.97,0.78,0.46));
#8132=CARTESIAN_POINT('',(-3.07,1.7,0.46));
#8133=CARTESIAN_POINT('',(-3.07,0.78,0.46));
#8134=CARTESIAN_POINT('',(-1.97,1.7,0.46));
#8135=CARTESIAN_POINT('Origin',(-1.97,1.7,2.3));
#8136=CARTESIAN_POINT('',(-1.97,1.7,2.3));
#8137=CARTESIAN_POINT('',(-1.97,1.7,0.46));
#8138=CARTESIAN_POINT('',(-3.07,1.7,2.3));
#8139=CARTESIAN_POINT('',(-3.07,1.7,0.46));
#8140=CARTESIAN_POINT('',(-1.97,1.7,2.3));
#8141=CARTESIAN_POINT('Origin',(-1.97,-1.7,2.3));
#8142=CARTESIAN_POINT('',(-1.97,-1.7,2.3));
#8143=CARTESIAN_POINT('',(-1.97,1.7,2.3));
#8144=CARTESIAN_POINT('',(-3.07,-1.7,2.3));
#8145=CARTESIAN_POINT('',(-3.07,1.7,2.3));
#8146=CARTESIAN_POINT('',(-1.97,-1.7,2.3));
#8147=CARTESIAN_POINT('Origin',(-1.97,-1.7,0.46));
#8148=CARTESIAN_POINT('',(-1.97,-1.7,2.3));
#8149=CARTESIAN_POINT('',(-3.07,-1.7,2.3));
#8150=CARTESIAN_POINT('Origin',(-1.97,0.,1.38));
#8151=CARTESIAN_POINT('Origin',(-3.07,0.,1.38));
#8152=CARTESIAN_POINT('',(0.,0.,0.));
#8153=CARTESIAN_POINT('',(0.,0.,0.));
#8154=CARTESIAN_POINT('',(0.,0.,0.));
#8155=CARTESIAN_POINT('',(0.,0.,0.));
#8156=CARTESIAN_POINT('Origin',(11.,3.5,5.1));
#8157=CARTESIAN_POINT('',(10.835,3.5,5.2));
#8158=CARTESIAN_POINT('Origin',(11.,3.5,5.2));
#8159=CARTESIAN_POINT('',(10.835,3.5,6.4));
#8160=CARTESIAN_POINT('',(10.835,3.5,5.1));
#8161=CARTESIAN_POINT('Origin',(11.,3.5,6.4));
#8162=CARTESIAN_POINT('Origin',(11.,0.,5.1));
#8163=CARTESIAN_POINT('',(10.75,-3.06161699786838E-17,5.2));
#8164=CARTESIAN_POINT('Origin',(11.,0.,5.2));
#8165=CARTESIAN_POINT('',(10.75,3.06161699786838E-17,6.4));
#8166=CARTESIAN_POINT('',(10.75,-3.06161699786838E-17,5.1));
#8167=CARTESIAN_POINT('Origin',(11.,0.,6.4));
#8168=CARTESIAN_POINT('Origin',(12.5,-1.9,5.1));
#8169=CARTESIAN_POINT('',(12.225,-1.9,5.2));
#8170=CARTESIAN_POINT('Origin',(12.5,-1.9,5.2));
#8171=CARTESIAN_POINT('',(12.225,-1.9,6.4));
#8172=CARTESIAN_POINT('',(12.225,-1.9,5.1));
#8173=CARTESIAN_POINT('Origin',(12.5,-1.9,6.4));
#8174=CARTESIAN_POINT('Origin',(9.5,1.9,5.1));
#8175=CARTESIAN_POINT('',(9.225,1.9,5.2));
#8176=CARTESIAN_POINT('Origin',(9.5,1.9,5.2));
#8177=CARTESIAN_POINT('',(9.225,1.9,6.4));
#8178=CARTESIAN_POINT('',(9.225,1.9,5.1));
#8179=CARTESIAN_POINT('Origin',(9.5,1.9,6.4));
#8180=CARTESIAN_POINT('Origin',(9.5,-1.9,5.1));
#8181=CARTESIAN_POINT('',(9.225,-1.9,5.2));
#8182=CARTESIAN_POINT('Origin',(9.5,-1.9,5.2));
#8183=CARTESIAN_POINT('',(9.225,-1.9,6.4));
#8184=CARTESIAN_POINT('',(9.225,-1.9,5.1));
#8185=CARTESIAN_POINT('Origin',(9.5,-1.9,6.4));
#8186=CARTESIAN_POINT('Origin',(12.5,1.9,5.1));
#8187=CARTESIAN_POINT('',(12.225,1.9,5.2));
#8188=CARTESIAN_POINT('Origin',(12.5,1.9,5.2));
#8189=CARTESIAN_POINT('',(12.225,1.9,6.4));
#8190=CARTESIAN_POINT('',(12.225,1.9,5.1));
#8191=CARTESIAN_POINT('Origin',(12.5,1.9,6.4));
#8192=CARTESIAN_POINT('Origin',(15.,4.,5.2));
#8193=CARTESIAN_POINT('',(15.,4.,5.2));
#8194=CARTESIAN_POINT('',(7.,4.,5.2));
#8195=CARTESIAN_POINT('',(15.,4.,5.2));
#8196=CARTESIAN_POINT('',(7.,4.,6.4));
#8197=CARTESIAN_POINT('',(7.,4.,5.2));
#8198=CARTESIAN_POINT('',(15.,4.,6.4));
#8199=CARTESIAN_POINT('',(15.,4.,6.4));
#8200=CARTESIAN_POINT('',(15.,4.,5.2));
#8201=CARTESIAN_POINT('Origin',(15.,-4.,5.2));
#8202=CARTESIAN_POINT('',(15.,-4.,5.2));
#8203=CARTESIAN_POINT('',(15.,-4.,5.2));
#8204=CARTESIAN_POINT('',(15.,-4.,6.4));
#8205=CARTESIAN_POINT('',(15.,-4.,6.4));
#8206=CARTESIAN_POINT('',(15.,-4.,5.2));
#8207=CARTESIAN_POINT('Origin',(7.,-4.,5.2));
#8208=CARTESIAN_POINT('',(7.,-4.,5.2));
#8209=CARTESIAN_POINT('',(7.,-4.,5.2));
#8210=CARTESIAN_POINT('',(7.,-4.,6.4));
#8211=CARTESIAN_POINT('',(7.,-4.,6.4));
#8212=CARTESIAN_POINT('',(7.,-4.,5.2));
#8213=CARTESIAN_POINT('Origin',(7.,4.,5.2));
#8214=CARTESIAN_POINT('',(7.,4.,5.2));
#8215=CARTESIAN_POINT('',(7.,4.,6.4));
#8216=CARTESIAN_POINT('Origin',(11.,0.,6.4));
#8217=CARTESIAN_POINT('Origin',(11.,0.,5.2));
#8218=CARTESIAN_POINT('',(0.,0.,0.));
#8219=CARTESIAN_POINT('Origin',(11.,0.,6.4));
#8220=CARTESIAN_POINT('',(10.67,-4.04133443718627E-17,8.4));
#8221=CARTESIAN_POINT('Origin',(11.,0.,8.4));
#8222=CARTESIAN_POINT('',(10.67,-4.04133443718627E-17,6.4));
#8223=CARTESIAN_POINT('',(10.67,-4.04133443718627E-17,6.4));
#8224=CARTESIAN_POINT('Origin',(11.,0.,6.4));
#8225=CARTESIAN_POINT('Origin',(11.,0.,6.4));
#8226=CARTESIAN_POINT('',(9.5,-1.83697019872103E-16,8.4));
#8227=CARTESIAN_POINT('Origin',(11.,0.,8.4));
#8228=CARTESIAN_POINT('',(9.5,-1.83697019872103E-16,6.4));
#8229=CARTESIAN_POINT('',(9.5,-1.83697019872103E-16,6.4));
#8230=CARTESIAN_POINT('Origin',(11.,0.,6.4));
#8231=CARTESIAN_POINT('Origin',(11.,0.,8.4));
#8232=CARTESIAN_POINT('Origin',(11.,0.,6.4));
#8233=CARTESIAN_POINT('',(0.,0.,0.));
#8234=CARTESIAN_POINT('Origin',(0.,0.09,0.));
#8235=CARTESIAN_POINT('',(-0.285,0.1,3.49024337756996E-17));
#8236=CARTESIAN_POINT('Origin',(0.,0.1,0.));
#8237=CARTESIAN_POINT('',(-0.265,0.08,-3.24531401774049E-17));
#8238=CARTESIAN_POINT('',(-0.275,0.09,3.36777869765522E-17));
#8239=CARTESIAN_POINT('Origin',(0.,0.08,0.));
#8240=CARTESIAN_POINT('Origin',(0.,0.,0.));
#8241=CARTESIAN_POINT('',(-0.265,0.,3.24531401774049E-17));
#8242=CARTESIAN_POINT('',(-0.265,0.,3.24531401774049E-17));
#8243=CARTESIAN_POINT('Origin',(0.,0.,0.));
#8244=CARTESIAN_POINT('Origin',(0.,0.1,0.));
#8245=CARTESIAN_POINT('',(-0.5,0.1,6.12323399573677E-17));
#8246=CARTESIAN_POINT('Origin',(0.,0.1,0.));
#8247=CARTESIAN_POINT('Origin',(0.,0.,0.));
#8248=CARTESIAN_POINT('',(-0.5,0.,6.12323399573677E-17));
#8249=CARTESIAN_POINT('',(-0.5,0.,6.12323399573677E-17));
#8250=CARTESIAN_POINT('Origin',(0.,0.,0.));
#8251=CARTESIAN_POINT('Origin',(0.,0.,0.));
#8252=CARTESIAN_POINT('',(0.,0.,0.));
#8253=CARTESIAN_POINT('Origin',(0.375,0.5,0.));
#8254=CARTESIAN_POINT('',(-0.375,0.5,-4.59242549680257E-17));
#8255=CARTESIAN_POINT('Origin',(0.,0.5,0.));
#8256=CARTESIAN_POINT('Origin',(0.,0.475,0.));
#8257=CARTESIAN_POINT('',(-0.425,0.45,-5.20474889637625E-17));
#8258=CARTESIAN_POINT('Origin',(0.,0.45,0.));
#8259=CARTESIAN_POINT('',(-0.4,0.475,-4.89858719658941E-17));
#8260=CARTESIAN_POINT('Origin',(0.,0.24,0.));
#8261=CARTESIAN_POINT('',(-0.425,0.0299999999999998,-5.20474889637625E-17));
#8262=CARTESIAN_POINT('Origin',(0.,0.0299999999999998,0.));
#8263=CARTESIAN_POINT('',(-0.425,0.24,-5.20474889637625E-17));
#8264=CARTESIAN_POINT('Origin',(0.,0.0150000000000001,0.));
#8265=CARTESIAN_POINT('',(-0.395,4.85722573273506E-17,-4.83735485663204E-17));
#8266=CARTESIAN_POINT('Origin',(0.,0.,0.));
#8267=CARTESIAN_POINT('',(-0.41,0.0150000000000001,-5.02105187650415E-17));
#8268=CARTESIAN_POINT('Origin',(0.27,0.,0.));
#8269=CARTESIAN_POINT('',(-0.27,0.,-3.30654635769785E-17));
#8270=CARTESIAN_POINT('Origin',(0.,0.,0.));
#8271=CARTESIAN_POINT('Origin',(0.,-0.02,0.));
#8272=CARTESIAN_POINT('',(-0.24505,-0.0498999999999999,3.00099698131059E-17));
#8273=CARTESIAN_POINT('Origin',(0.,-0.0498999999999999,0.));
#8274=CARTESIAN_POINT('',(-0.26,-0.02,-3.18408167778312E-17));
#8275=CARTESIAN_POINT('Origin',(0.,-0.995,0.));
#8276=CARTESIAN_POINT('',(-0.24505,-1.95495,3.00099698131059E-17));
#8277=CARTESIAN_POINT('Origin',(0.,-1.95495,0.));
#8278=CARTESIAN_POINT('',(-0.24505,-0.995,-3.00099698131059E-17));
#8279=CARTESIAN_POINT('Origin',(0.,-1.975,0.));
#8280=CARTESIAN_POINT('',(-0.2,-2.,-2.44929359829471E-17));
#8281=CARTESIAN_POINT('Origin',(0.,-2.,0.));
#8282=CARTESIAN_POINT('',(-0.225,-1.975,-2.75545529808154E-17));
#8283=CARTESIAN_POINT('Origin',(0.,-2.,0.));
#8284=CARTESIAN_POINT('Origin',(0.115470053837925,-0.5,-0.2));
#8285=CARTESIAN_POINT('',(0.23094010767585,-0.5,0.));
#8286=CARTESIAN_POINT('',(0.115470053837925,-0.5,-0.2));
#8287=CARTESIAN_POINT('',(0.23094010767585,-0.5,0.));
#8288=CARTESIAN_POINT('',(0.115470053837925,-0.8,-0.2));
#8289=CARTESIAN_POINT('',(0.115470053837925,-0.5,-0.2));
#8290=CARTESIAN_POINT('',(0.23094010767585,-0.8,0.));
#8291=CARTESIAN_POINT('',(0.23094010767585,-0.8,0.));
#8292=CARTESIAN_POINT('',(0.23094010767585,-0.5,0.));
#8293=CARTESIAN_POINT('Origin',(-0.115470053837925,-0.5,-0.2));
#8294=CARTESIAN_POINT('',(-0.115470053837925,-0.5,-0.2));
#8295=CARTESIAN_POINT('',(0.115470053837925,-0.5,-0.2));
#8296=CARTESIAN_POINT('',(-0.115470053837925,-0.8,-0.2));
#8297=CARTESIAN_POINT('',(-0.115470053837925,-0.5,-0.2));
#8298=CARTESIAN_POINT('',(0.115470053837925,-0.8,-0.2));
#8299=CARTESIAN_POINT('Origin',(-0.23094010767585,-0.5,-2.77555756156289E-17));
#8300=CARTESIAN_POINT('',(-0.23094010767585,-0.5,-2.82820063659975E-17));
#8301=CARTESIAN_POINT('',(-0.115470053837925,-0.5,-0.2));
#8302=CARTESIAN_POINT('',(-0.23094010767585,-0.8,-2.77555756156289E-17));
#8303=CARTESIAN_POINT('',(-0.23094010767585,-0.5,-2.82820063659975E-17));
#8304=CARTESIAN_POINT('',(-0.115470053837925,-0.8,-0.2));
#8305=CARTESIAN_POINT('Origin',(-0.115470053837925,-0.5,0.2));
#8306=CARTESIAN_POINT('',(-0.115470053837925,-0.5,0.2));
#8307=CARTESIAN_POINT('',(-0.23094010767585,-0.5,-2.82820063659975E-17));
#8308=CARTESIAN_POINT('',(-0.115470053837925,-0.8,0.2));
#8309=CARTESIAN_POINT('',(-0.115470053837925,-0.5,0.2));
#8310=CARTESIAN_POINT('',(-0.23094010767585,-0.8,-2.82820063659975E-17));
#8311=CARTESIAN_POINT('Origin',(0.115470053837925,-0.5,0.2));
#8312=CARTESIAN_POINT('',(0.115470053837925,-0.5,0.2));
#8313=CARTESIAN_POINT('',(-0.115470053837925,-0.5,0.2));
#8314=CARTESIAN_POINT('',(0.115470053837925,-0.8,0.2));
#8315=CARTESIAN_POINT('',(0.115470053837925,-0.5,0.2));
#8316=CARTESIAN_POINT('',(-0.115470053837925,-0.8,0.2));
#8317=CARTESIAN_POINT('Origin',(0.23094010767585,-0.5,0.));
#8318=CARTESIAN_POINT('',(0.115470053837925,-0.5,0.2));
#8319=CARTESIAN_POINT('',(0.115470053837925,-0.8,0.2));
#8320=CARTESIAN_POINT('Origin',(0.,-0.5,0.));
#8321=CARTESIAN_POINT('Origin',(0.,-0.8,0.));
#8322=CARTESIAN_POINT('',(0.,0.,0.));
#8323=CARTESIAN_POINT('',(-4.,-3.5,1.));
#8324=CARTESIAN_POINT('',(-4.,3.5,1.));
#8325=CARTESIAN_POINT('',(2.5,-3.5,1.42));
#8326=CARTESIAN_POINT('',(2.5,-3.5,2.8));
#8327=CARTESIAN_POINT('',(2.5,-3.5,2.9));
#8328=CARTESIAN_POINT('',(2.5,3.5,1.42));
#8329=CARTESIAN_POINT('',(2.5,3.5,2.8));
#8330=CARTESIAN_POINT('',(2.5,3.5,2.9));
#8331=CARTESIAN_POINT('',(19.5,-3.5,1.42));
#8332=CARTESIAN_POINT('',(19.5,-3.5,2.8));
#8333=CARTESIAN_POINT('',(19.5,-3.5,2.9));
#8334=CARTESIAN_POINT('',(19.5,3.5,1.42));
#8335=CARTESIAN_POINT('',(19.5,3.5,2.8));
#8336=CARTESIAN_POINT('',(19.5,3.5,2.9));
#8337=CARTESIAN_POINT('',(0.,0.,2.8));
#8338=CARTESIAN_POINT('',(2.,0.,3.77));
#8339=CARTESIAN_POINT('',(8.,0.,3.77));
#8340=CARTESIAN_POINT('',(14.,0.,3.77));
#8341=CARTESIAN_POINT('',(20.,0.,3.77));
#8342=CARTESIAN_POINT('',(0.,0.,0.));
#8343=CARTESIAN_POINT('',(-1.,-2.4,4.));
#8344=CARTESIAN_POINT('',(-1.,2.4,4.));
#8345=CARTESIAN_POINT('',(24.,0.,0.));
#8346=CARTESIAN_POINT('',(23.,-2.4,4.));
#8347=CARTESIAN_POINT('',(23.,2.4,4.));
#8348=CARTESIAN_POINT('',(0.,0.,0.));
#8349=CARTESIAN_POINT('',(21.8,0.,0.));
#8350=CARTESIAN_POINT('',(0.,0.,0.));
#8351=CARTESIAN_POINT('',(0.,7.,0.));
#8352=CARTESIAN_POINT('',(16.,0.,0.));
#8353=CARTESIAN_POINT('',(16.,7.,0.));
#8354=CARTESIAN_POINT('',(0.,0.,0.));
#8355=CARTESIAN_POINT('Origin',(0.,0.,0.));
#8356=CARTESIAN_POINT('',(-0.32,0.16,3.91886975727153E-17));
#8357=CARTESIAN_POINT('Origin',(0.,0.16,0.));
#8358=CARTESIAN_POINT('',(-0.32,0.,3.91886975727153E-17));
#8359=CARTESIAN_POINT('',(-0.32,0.,3.91886975727153E-17));
#8360=CARTESIAN_POINT('Origin',(0.,0.,0.));
#8361=CARTESIAN_POINT('Origin',(0.,0.,0.));
#8362=CARTESIAN_POINT('',(-0.6,0.16,7.34788079488412E-17));
#8363=CARTESIAN_POINT('Origin',(0.,0.16,0.));
#8364=CARTESIAN_POINT('',(-0.6,0.,7.34788079488412E-17));
#8365=CARTESIAN_POINT('',(-0.6,0.,7.34788079488412E-17));
#8366=CARTESIAN_POINT('Origin',(0.,0.,0.));
#8367=CARTESIAN_POINT('Origin',(0.,0.16,0.));
#8368=CARTESIAN_POINT('Origin',(0.,0.,0.));
#8369=CARTESIAN_POINT('',(0.,0.,0.));
#8370=CARTESIAN_POINT('Origin',(0.45,0.6,0.));
#8371=CARTESIAN_POINT('',(-0.45,0.6,-5.51091059616309E-17));
#8372=CARTESIAN_POINT('Origin',(0.,0.6,0.));
#8373=CARTESIAN_POINT('Origin',(0.,0.575,0.));
#8374=CARTESIAN_POINT('',(-0.5,0.55,-6.12323399573677E-17));
#8375=CARTESIAN_POINT('Origin',(0.,0.55,0.));
#8376=CARTESIAN_POINT('',(-0.475,0.575,-5.81707229594993E-17));
#8377=CARTESIAN_POINT('Origin',(0.,0.29,0.));
#8378=CARTESIAN_POINT('',(-0.5,0.0299999999999998,-6.12323399573677E-17));
#8379=CARTESIAN_POINT('Origin',(0.,0.0299999999999998,0.));
#8380=CARTESIAN_POINT('',(-0.5,0.29,-6.12323399573677E-17));
#8381=CARTESIAN_POINT('Origin',(0.,0.0150000000000001,0.));
#8382=CARTESIAN_POINT('',(-0.47,7.11236625150491E-17,-5.75583995599256E-17));
#8383=CARTESIAN_POINT('Origin',(0.,0.,0.));
#8384=CARTESIAN_POINT('',(-0.485,0.0150000000000001,-5.93953697586466E-17));
#8385=CARTESIAN_POINT('Origin',(0.32,0.,0.));
#8386=CARTESIAN_POINT('',(-0.32,-6.93889390390723E-18,-3.91886975727153E-17));
#8387=CARTESIAN_POINT('Origin',(0.,0.,0.));
#8388=CARTESIAN_POINT('Origin',(0.,-0.02,0.));
#8389=CARTESIAN_POINT('',(-0.2942,-0.0515999999999999,3.60291088309151E-17));
#8390=CARTESIAN_POINT('Origin',(0.,-0.0515999999999999,0.));
#8391=CARTESIAN_POINT('',(-0.31,-0.02,-3.7964050773568E-17));
#8392=CARTESIAN_POINT('Origin',(0.,-1.24,0.));
#8393=CARTESIAN_POINT('',(-0.2942,-2.4458,3.60291088309151E-17));
#8394=CARTESIAN_POINT('Origin',(0.,-2.4458,0.));
#8395=CARTESIAN_POINT('',(-0.2942,-1.24,-3.60291088309151E-17));
#8396=CARTESIAN_POINT('Origin',(0.,-2.47,0.));
#8397=CARTESIAN_POINT('',(-0.24,-2.5,-2.93915231795365E-17));
#8398=CARTESIAN_POINT('Origin',(0.,-2.5,0.));
#8399=CARTESIAN_POINT('',(-0.27,-2.47,-3.30654635769785E-17));
#8400=CARTESIAN_POINT('Origin',(0.,-2.5,0.));
#8401=CARTESIAN_POINT('Origin',(0.144337567297406,-0.6,-0.25));
#8402=CARTESIAN_POINT('',(0.288675134594813,-0.6,0.));
#8403=CARTESIAN_POINT('',(0.144337567297406,-0.6,-0.25));
#8404=CARTESIAN_POINT('',(0.288675134594813,-0.6,0.));
#8405=CARTESIAN_POINT('',(0.144337567297406,-0.96,-0.25));
#8406=CARTESIAN_POINT('',(0.144337567297406,-0.6,-0.25));
#8407=CARTESIAN_POINT('',(0.288675134594813,-0.96,0.));
#8408=CARTESIAN_POINT('',(0.288675134594813,-0.96,0.));
#8409=CARTESIAN_POINT('',(0.288675134594813,-0.6,0.));
#8410=CARTESIAN_POINT('Origin',(-0.144337567297406,-0.6,-0.25));
#8411=CARTESIAN_POINT('',(-0.144337567297406,-0.6,-0.25));
#8412=CARTESIAN_POINT('',(0.144337567297406,-0.6,-0.25));
#8413=CARTESIAN_POINT('',(-0.144337567297406,-0.96,-0.25));
#8414=CARTESIAN_POINT('',(-0.144337567297406,-0.6,-0.25));
#8415=CARTESIAN_POINT('',(0.144337567297406,-0.96,-0.25));
#8416=CARTESIAN_POINT('Origin',(-0.288675134594813,-0.6,-8.32667268468867E-17));
#8417=CARTESIAN_POINT('',(-0.288675134594813,-0.6,-3.53525079574969E-17));
#8418=CARTESIAN_POINT('',(-0.144337567297406,-0.6,-0.25));
#8419=CARTESIAN_POINT('',(-0.288675134594813,-0.96,-5.55111512312578E-17));
#8420=CARTESIAN_POINT('',(-0.288675134594813,-0.6,-3.53525079574969E-17));
#8421=CARTESIAN_POINT('',(-0.144337567297406,-0.96,-0.25));
#8422=CARTESIAN_POINT('Origin',(-0.144337567297407,-0.6,0.25));
#8423=CARTESIAN_POINT('',(-0.144337567297407,-0.6,0.25));
#8424=CARTESIAN_POINT('',(-0.288675134594813,-0.6,-3.53525079574969E-17));
#8425=CARTESIAN_POINT('',(-0.144337567297407,-0.96,0.25));
#8426=CARTESIAN_POINT('',(-0.144337567297407,-0.6,0.25));
#8427=CARTESIAN_POINT('',(-0.288675134594813,-0.96,-3.53525079574969E-17));
#8428=CARTESIAN_POINT('Origin',(0.144337567297406,-0.6,0.25));
#8429=CARTESIAN_POINT('',(0.144337567297406,-0.6,0.25));
#8430=CARTESIAN_POINT('',(-0.144337567297407,-0.6,0.25));
#8431=CARTESIAN_POINT('',(0.144337567297406,-0.96,0.25));
#8432=CARTESIAN_POINT('',(0.144337567297406,-0.6,0.25));
#8433=CARTESIAN_POINT('',(-0.144337567297407,-0.96,0.25));
#8434=CARTESIAN_POINT('Origin',(0.288675134594813,-0.6,0.));
#8435=CARTESIAN_POINT('',(0.144337567297406,-0.6,0.25));
#8436=CARTESIAN_POINT('',(0.144337567297406,-0.96,0.25));
#8437=CARTESIAN_POINT('Origin',(0.,-0.6,0.));
#8438=CARTESIAN_POINT('Origin',(0.,-0.96,0.));
#8439=CARTESIAN_POINT('',(11.,0.,2.8));
#8440=CARTESIAN_POINT('',(0.,0.,0.));
#8441=CARTESIAN_POINT('',(0.,0.,0.));
#8442=CARTESIAN_POINT('',(9.5,-1.9,6.4));
#8443=CARTESIAN_POINT('',(9.5,-1.9,6.5));
#8444=CARTESIAN_POINT('',(9.5,1.9,6.4));
#8445=CARTESIAN_POINT('',(9.5,1.9,6.5));
#8446=CARTESIAN_POINT('',(12.5,-1.9,6.4));
#8447=CARTESIAN_POINT('',(12.5,-1.9,6.5));
#8448=CARTESIAN_POINT('',(12.5,1.9,6.4));
#8449=CARTESIAN_POINT('',(12.5,1.9,6.5));
#8450=CARTESIAN_POINT('',(11.,0.,8.4));
#8451=CARTESIAN_POINT('',(11.,0.,8.56));
#8452=CARTESIAN_POINT('',(0.,0.,0.));
#8453=CARTESIAN_POINT('',(0.,0.,0.));
#8454=UNCERTAINTY_MEASURE_WITH_UNIT(LENGTH_MEASURE(0.001),#8500,
'DISTANCE_ACCURACY_VALUE',
'Maximum model space distance between geometric entities at asserted c
onnectivities');
#8455=UNCERTAINTY_MEASURE_WITH_UNIT(LENGTH_MEASURE(0.001),#8500,
'DISTANCE_ACCURACY_VALUE',
'Maximum model space distance between geometric entities at asserted c
onnectivities');
#8456=UNCERTAINTY_MEASURE_WITH_UNIT(LENGTH_MEASURE(0.001),#8500,
'DISTANCE_ACCURACY_VALUE',
'Maximum model space distance between geometric entities at asserted c
onnectivities');
#8457=UNCERTAINTY_MEASURE_WITH_UNIT(LENGTH_MEASURE(0.001),#8500,
'DISTANCE_ACCURACY_VALUE',
'Maximum model space distance between geometric entities at asserted c
onnectivities');
#8458=UNCERTAINTY_MEASURE_WITH_UNIT(LENGTH_MEASURE(0.001),#8500,
'DISTANCE_ACCURACY_VALUE',
'Maximum model space distance between geometric entities at asserted c
onnectivities');
#8459=UNCERTAINTY_MEASURE_WITH_UNIT(LENGTH_MEASURE(0.001),#8500,
'DISTANCE_ACCURACY_VALUE',
'Maximum model space distance between geometric entities at asserted c
onnectivities');
#8460=UNCERTAINTY_MEASURE_WITH_UNIT(LENGTH_MEASURE(0.001),#8500,
'DISTANCE_ACCURACY_VALUE',
'Maximum model space distance between geometric entities at asserted c
onnectivities');
#8461=UNCERTAINTY_MEASURE_WITH_UNIT(LENGTH_MEASURE(0.001),#8500,
'DISTANCE_ACCURACY_VALUE',
'Maximum model space distance between geometric entities at asserted c
onnectivities');
#8462=UNCERTAINTY_MEASURE_WITH_UNIT(LENGTH_MEASURE(0.001),#8500,
'DISTANCE_ACCURACY_VALUE',
'Maximum model space distance between geometric entities at asserted c
onnectivities');
#8463=UNCERTAINTY_MEASURE_WITH_UNIT(LENGTH_MEASURE(0.001),#8500,
'DISTANCE_ACCURACY_VALUE',
'Maximum model space distance between geometric entities at asserted c
onnectivities');
#8464=UNCERTAINTY_MEASURE_WITH_UNIT(LENGTH_MEASURE(0.001),#8500,
'DISTANCE_ACCURACY_VALUE',
'Maximum model space distance between geometric entities at asserted c
onnectivities');
#8465=UNCERTAINTY_MEASURE_WITH_UNIT(LENGTH_MEASURE(0.001),#8500,
'DISTANCE_ACCURACY_VALUE',
'Maximum model space distance between geometric entities at asserted c
onnectivities');
#8466=UNCERTAINTY_MEASURE_WITH_UNIT(LENGTH_MEASURE(0.001),#8500,
'DISTANCE_ACCURACY_VALUE',
'Maximum model space distance between geometric entities at asserted c
onnectivities');
#8467=UNCERTAINTY_MEASURE_WITH_UNIT(LENGTH_MEASURE(0.001),#8500,
'DISTANCE_ACCURACY_VALUE',
'Maximum model space distance between geometric entities at asserted c
onnectivities');
#8468=UNCERTAINTY_MEASURE_WITH_UNIT(LENGTH_MEASURE(0.001),#8500,
'DISTANCE_ACCURACY_VALUE',
'Maximum model space distance between geometric entities at asserted c
onnectivities');
#8469=UNCERTAINTY_MEASURE_WITH_UNIT(LENGTH_MEASURE(0.001),#8500,
'DISTANCE_ACCURACY_VALUE',
'Maximum model space distance between geometric entities at asserted c
onnectivities');
#8470=UNCERTAINTY_MEASURE_WITH_UNIT(LENGTH_MEASURE(0.001),#8500,
'DISTANCE_ACCURACY_VALUE',
'Maximum model space distance between geometric entities at asserted c
onnectivities');
#8471=UNCERTAINTY_MEASURE_WITH_UNIT(LENGTH_MEASURE(0.001),#8500,
'DISTANCE_ACCURACY_VALUE',
'Maximum model space distance between geometric entities at asserted c
onnectivities');
#8472=UNCERTAINTY_MEASURE_WITH_UNIT(LENGTH_MEASURE(0.001),#8500,
'DISTANCE_ACCURACY_VALUE',
'Maximum model space distance between geometric entities at asserted c
onnectivities');
#8473=UNCERTAINTY_MEASURE_WITH_UNIT(LENGTH_MEASURE(0.001),#8500,
'DISTANCE_ACCURACY_VALUE',
'Maximum model space distance between geometric entities at asserted c
onnectivities');
#8474=UNCERTAINTY_MEASURE_WITH_UNIT(LENGTH_MEASURE(0.001),#8500,
'DISTANCE_ACCURACY_VALUE',
'Maximum model space distance between geometric entities at asserted c
onnectivities');
#8475=UNCERTAINTY_MEASURE_WITH_UNIT(LENGTH_MEASURE(0.001),#8500,
'DISTANCE_ACCURACY_VALUE',
'Maximum model space distance between geometric entities at asserted c
onnectivities');
#8476=UNCERTAINTY_MEASURE_WITH_UNIT(LENGTH_MEASURE(0.001),#8500,
'DISTANCE_ACCURACY_VALUE',
'Maximum model space distance between geometric entities at asserted c
onnectivities');
#8477=(
GEOMETRIC_REPRESENTATION_CONTEXT(3)
GLOBAL_UNCERTAINTY_ASSIGNED_CONTEXT((#8454))
GLOBAL_UNIT_ASSIGNED_CONTEXT((#8500,#8502,#8503))
REPRESENTATION_CONTEXT('','3D')
);
#8478=(
GEOMETRIC_REPRESENTATION_CONTEXT(3)
GLOBAL_UNCERTAINTY_ASSIGNED_CONTEXT((#8455))
GLOBAL_UNIT_ASSIGNED_CONTEXT((#8500,#8502,#8503))
REPRESENTATION_CONTEXT('','3D')
);
#8479=(
GEOMETRIC_REPRESENTATION_CONTEXT(3)
GLOBAL_UNCERTAINTY_ASSIGNED_CONTEXT((#8456))
GLOBAL_UNIT_ASSIGNED_CONTEXT((#8500,#8502,#8503))
REPRESENTATION_CONTEXT('','3D')
);
#8480=(
GEOMETRIC_REPRESENTATION_CONTEXT(3)
GLOBAL_UNCERTAINTY_ASSIGNED_CONTEXT((#8457))
GLOBAL_UNIT_ASSIGNED_CONTEXT((#8500,#8502,#8503))
REPRESENTATION_CONTEXT('','3D')
);
#8481=(
GEOMETRIC_REPRESENTATION_CONTEXT(3)
GLOBAL_UNCERTAINTY_ASSIGNED_CONTEXT((#8458))
GLOBAL_UNIT_ASSIGNED_CONTEXT((#8500,#8502,#8503))
REPRESENTATION_CONTEXT('','3D')
);
#8482=(
GEOMETRIC_REPRESENTATION_CONTEXT(3)
GLOBAL_UNCERTAINTY_ASSIGNED_CONTEXT((#8459))
GLOBAL_UNIT_ASSIGNED_CONTEXT((#8500,#8502,#8503))
REPRESENTATION_CONTEXT('','3D')
);
#8483=(
GEOMETRIC_REPRESENTATION_CONTEXT(3)
GLOBAL_UNCERTAINTY_ASSIGNED_CONTEXT((#8460))
GLOBAL_UNIT_ASSIGNED_CONTEXT((#8500,#8502,#8503))
REPRESENTATION_CONTEXT('','3D')
);
#8484=(
GEOMETRIC_REPRESENTATION_CONTEXT(3)
GLOBAL_UNCERTAINTY_ASSIGNED_CONTEXT((#8461))
GLOBAL_UNIT_ASSIGNED_CONTEXT((#8500,#8502,#8503))
REPRESENTATION_CONTEXT('','3D')
);
#8485=(
GEOMETRIC_REPRESENTATION_CONTEXT(3)
GLOBAL_UNCERTAINTY_ASSIGNED_CONTEXT((#8462))
GLOBAL_UNIT_ASSIGNED_CONTEXT((#8500,#8502,#8503))
REPRESENTATION_CONTEXT('','3D')
);
#8486=(
GEOMETRIC_REPRESENTATION_CONTEXT(3)
GLOBAL_UNCERTAINTY_ASSIGNED_CONTEXT((#8463))
GLOBAL_UNIT_ASSIGNED_CONTEXT((#8500,#8502,#8503))
REPRESENTATION_CONTEXT('','3D')
);
#8487=(
GEOMETRIC_REPRESENTATION_CONTEXT(3)
GLOBAL_UNCERTAINTY_ASSIGNED_CONTEXT((#8464))
GLOBAL_UNIT_ASSIGNED_CONTEXT((#8500,#8502,#8503))
REPRESENTATION_CONTEXT('','3D')
);
#8488=(
GEOMETRIC_REPRESENTATION_CONTEXT(3)
GLOBAL_UNCERTAINTY_ASSIGNED_CONTEXT((#8465))
GLOBAL_UNIT_ASSIGNED_CONTEXT((#8500,#8502,#8503))
REPRESENTATION_CONTEXT('','3D')
);
#8489=(
GEOMETRIC_REPRESENTATION_CONTEXT(3)
GLOBAL_UNCERTAINTY_ASSIGNED_CONTEXT((#8466))
GLOBAL_UNIT_ASSIGNED_CONTEXT((#8500,#8502,#8503))
REPRESENTATION_CONTEXT('','3D')
);
#8490=(
GEOMETRIC_REPRESENTATION_CONTEXT(3)
GLOBAL_UNCERTAINTY_ASSIGNED_CONTEXT((#8467))
GLOBAL_UNIT_ASSIGNED_CONTEXT((#8500,#8502,#8503))
REPRESENTATION_CONTEXT('','3D')
);
#8491=(
GEOMETRIC_REPRESENTATION_CONTEXT(3)
GLOBAL_UNCERTAINTY_ASSIGNED_CONTEXT((#8468))
GLOBAL_UNIT_ASSIGNED_CONTEXT((#8500,#8502,#8503))
REPRESENTATION_CONTEXT('','3D')
);
#8492=(
GEOMETRIC_REPRESENTATION_CONTEXT(3)
GLOBAL_UNCERTAINTY_ASSIGNED_CONTEXT((#8469))
GLOBAL_UNIT_ASSIGNED_CONTEXT((#8500,#8502,#8503))
REPRESENTATION_CONTEXT('','3D')
);
#8493=(
GEOMETRIC_REPRESENTATION_CONTEXT(3)
GLOBAL_UNCERTAINTY_ASSIGNED_CONTEXT((#8470))
GLOBAL_UNIT_ASSIGNED_CONTEXT((#8500,#8502,#8503))
REPRESENTATION_CONTEXT('','3D')
);
#8494=(
GEOMETRIC_REPRESENTATION_CONTEXT(3)
GLOBAL_UNCERTAINTY_ASSIGNED_CONTEXT((#8471))
GLOBAL_UNIT_ASSIGNED_CONTEXT((#8500,#8502,#8503))
REPRESENTATION_CONTEXT('','3D')
);
#8495=(
GEOMETRIC_REPRESENTATION_CONTEXT(3)
GLOBAL_UNCERTAINTY_ASSIGNED_CONTEXT((#8472))
GLOBAL_UNIT_ASSIGNED_CONTEXT((#8500,#8502,#8503))
REPRESENTATION_CONTEXT('','3D')
);
#8496=(
GEOMETRIC_REPRESENTATION_CONTEXT(3)
GLOBAL_UNCERTAINTY_ASSIGNED_CONTEXT((#8473))
GLOBAL_UNIT_ASSIGNED_CONTEXT((#8500,#8502,#8503))
REPRESENTATION_CONTEXT('','3D')
);
#8497=(
GEOMETRIC_REPRESENTATION_CONTEXT(3)
GLOBAL_UNCERTAINTY_ASSIGNED_CONTEXT((#8474))
GLOBAL_UNIT_ASSIGNED_CONTEXT((#8500,#8502,#8503))
REPRESENTATION_CONTEXT('','3D')
);
#8498=(
GEOMETRIC_REPRESENTATION_CONTEXT(3)
GLOBAL_UNCERTAINTY_ASSIGNED_CONTEXT((#8475))
GLOBAL_UNIT_ASSIGNED_CONTEXT((#8500,#8502,#8503))
REPRESENTATION_CONTEXT('','3D')
);
#8499=(
GEOMETRIC_REPRESENTATION_CONTEXT(3)
GLOBAL_UNCERTAINTY_ASSIGNED_CONTEXT((#8476))
GLOBAL_UNIT_ASSIGNED_CONTEXT((#8500,#8502,#8503))
REPRESENTATION_CONTEXT('','3D')
);
#8500=(
LENGTH_UNIT()
NAMED_UNIT(*)
SI_UNIT(.CENTI.,.METRE.)
);
#8501=(
LENGTH_UNIT()
NAMED_UNIT(*)
SI_UNIT($,.METRE.)
);
#8502=(
NAMED_UNIT(*)
PLANE_ANGLE_UNIT()
SI_UNIT($,.RADIAN.)
);
#8503=(
NAMED_UNIT(*)
SI_UNIT($,.STERADIAN.)
SOLID_ANGLE_UNIT()
);
#8504=SHAPE_DEFINITION_REPRESENTATION(#8526,#8598);
#8505=SHAPE_DEFINITION_REPRESENTATION(#8527,#8599);
#8506=SHAPE_DEFINITION_REPRESENTATION(#8528,#8600);
#8507=SHAPE_DEFINITION_REPRESENTATION(#8529,#8601);
#8508=SHAPE_DEFINITION_REPRESENTATION(#8530,#8602);
#8509=SHAPE_DEFINITION_REPRESENTATION(#8531,#8603);
#8510=SHAPE_DEFINITION_REPRESENTATION(#8532,#8604);
#8511=SHAPE_DEFINITION_REPRESENTATION(#8533,#8605);
#8512=SHAPE_DEFINITION_REPRESENTATION(#8534,#8606);
#8513=SHAPE_DEFINITION_REPRESENTATION(#8535,#8607);
#8514=SHAPE_DEFINITION_REPRESENTATION(#8536,#8608);
#8515=SHAPE_DEFINITION_REPRESENTATION(#8537,#8609);
#8516=SHAPE_DEFINITION_REPRESENTATION(#8538,#8610);
#8517=SHAPE_DEFINITION_REPRESENTATION(#8539,#8611);
#8518=SHAPE_DEFINITION_REPRESENTATION(#8540,#8612);
#8519=SHAPE_DEFINITION_REPRESENTATION(#8541,#8613);
#8520=SHAPE_DEFINITION_REPRESENTATION(#8545,#8614);
#8521=SHAPE_DEFINITION_REPRESENTATION(#8546,#8615);
#8522=SHAPE_DEFINITION_REPRESENTATION(#8547,#8616);
#8523=SHAPE_DEFINITION_REPRESENTATION(#8548,#8617);
#8524=SHAPE_DEFINITION_REPRESENTATION(#8581,#8618);
#8525=SHAPE_DEFINITION_REPRESENTATION(#8582,#8619);
#8526=PRODUCT_DEFINITION_SHAPE('',$,#8621);
#8527=PRODUCT_DEFINITION_SHAPE('',$,#8622);
#8528=PRODUCT_DEFINITION_SHAPE('',$,#8623);
#8529=PRODUCT_DEFINITION_SHAPE('',$,#8624);
#8530=PRODUCT_DEFINITION_SHAPE('',$,#8625);
#8531=PRODUCT_DEFINITION_SHAPE('',$,#8626);
#8532=PRODUCT_DEFINITION_SHAPE('',$,#8627);
#8533=PRODUCT_DEFINITION_SHAPE('',$,#8628);
#8534=PRODUCT_DEFINITION_SHAPE('',$,#8629);
#8535=PRODUCT_DEFINITION_SHAPE('',$,#8630);
#8536=PRODUCT_DEFINITION_SHAPE('',$,#8631);
#8537=PRODUCT_DEFINITION_SHAPE('',$,#8632);
#8538=PRODUCT_DEFINITION_SHAPE('',$,#8633);
#8539=PRODUCT_DEFINITION_SHAPE('',$,#8634);
#8540=PRODUCT_DEFINITION_SHAPE('',$,#8635);
#8541=PRODUCT_DEFINITION_SHAPE('',$,#8636);
#8542=PRODUCT_DEFINITION_SHAPE($,$,#161);
#8543=PRODUCT_DEFINITION_SHAPE($,$,#162);
#8544=PRODUCT_DEFINITION_SHAPE($,$,#163);
#8545=PRODUCT_DEFINITION_SHAPE('',$,#8637);
#8546=PRODUCT_DEFINITION_SHAPE('',$,#8638);
#8547=PRODUCT_DEFINITION_SHAPE('',$,#8639);
#8548=PRODUCT_DEFINITION_SHAPE('',$,#8640);
#8549=PRODUCT_DEFINITION_SHAPE($,$,#164);
#8550=PRODUCT_DEFINITION_SHAPE($,$,#165);
#8551=PRODUCT_DEFINITION_SHAPE($,$,#166);
#8552=PRODUCT_DEFINITION_SHAPE($,$,#167);
#8553=PRODUCT_DEFINITION_SHAPE($,$,#168);
#8554=PRODUCT_DEFINITION_SHAPE($,$,#169);
#8555=PRODUCT_DEFINITION_SHAPE($,$,#170);
#8556=PRODUCT_DEFINITION_SHAPE($,$,#171);
#8557=PRODUCT_DEFINITION_SHAPE($,$,#172);
#8558=PRODUCT_DEFINITION_SHAPE($,$,#173);
#8559=PRODUCT_DEFINITION_SHAPE($,$,#174);
#8560=PRODUCT_DEFINITION_SHAPE($,$,#175);
#8561=PRODUCT_DEFINITION_SHAPE($,$,#176);
#8562=PRODUCT_DEFINITION_SHAPE($,$,#177);
#8563=PRODUCT_DEFINITION_SHAPE($,$,#178);
#8564=PRODUCT_DEFINITION_SHAPE($,$,#179);
#8565=PRODUCT_DEFINITION_SHAPE($,$,#180);
#8566=PRODUCT_DEFINITION_SHAPE($,$,#181);
#8567=PRODUCT_DEFINITION_SHAPE($,$,#182);
#8568=PRODUCT_DEFINITION_SHAPE($,$,#183);
#8569=PRODUCT_DEFINITION_SHAPE($,$,#184);
#8570=PRODUCT_DEFINITION_SHAPE($,$,#185);
#8571=PRODUCT_DEFINITION_SHAPE($,$,#186);
#8572=PRODUCT_DEFINITION_SHAPE($,$,#187);
#8573=PRODUCT_DEFINITION_SHAPE($,$,#188);
#8574=PRODUCT_DEFINITION_SHAPE($,$,#189);
#8575=PRODUCT_DEFINITION_SHAPE($,$,#190);
#8576=PRODUCT_DEFINITION_SHAPE($,$,#191);
#8577=PRODUCT_DEFINITION_SHAPE($,$,#192);
#8578=PRODUCT_DEFINITION_SHAPE($,$,#193);
#8579=PRODUCT_DEFINITION_SHAPE($,$,#194);
#8580=PRODUCT_DEFINITION_SHAPE($,$,#195);
#8581=PRODUCT_DEFINITION_SHAPE('',$,#8641);
#8582=PRODUCT_DEFINITION_SHAPE('',$,#8642);
#8583=PRODUCT_DEFINITION_SHAPE($,$,#196);
#8584=PRODUCT_DEFINITION_SHAPE($,$,#197);
#8585=PRODUCT_DEFINITION_SHAPE($,$,#198);
#8586=PRODUCT_DEFINITION_SHAPE($,$,#199);
#8587=PRODUCT_DEFINITION_SHAPE($,$,#200);
#8588=PRODUCT_DEFINITION_SHAPE($,$,#201);
#8589=PRODUCT_DEFINITION_SHAPE($,$,#202);
#8590=PRODUCT_DEFINITION_SHAPE($,$,#203);
#8591=PRODUCT_DEFINITION_SHAPE($,$,#204);
#8592=PRODUCT_DEFINITION_SHAPE($,$,#205);
#8593=PRODUCT_DEFINITION_SHAPE($,$,#206);
#8594=PRODUCT_DEFINITION_SHAPE($,$,#207);
#8595=PRODUCT_DEFINITION_SHAPE($,$,#208);
#8596=PRODUCT_DEFINITION_SHAPE($,$,#209);
#8597=PRODUCT_DEFINITION_SHAPE($,$,#210);
#8598=SHAPE_REPRESENTATION('',(#5162,#5629,#5630),#8477);
#8599=SHAPE_REPRESENTATION('',(#5163,#5549,#5550,#5551,#5552,#5553,#5554,
#5555,#5556,#5557,#5558,#5559,#5560,#5561,#5562,#5563,#5564,#5565,#5566,
#5567,#5568,#5569,#5570,#5571,#5572,#5573,#5574,#5575,#5576,#5577,#5578,
#5579,#5580),#8478);
#8600=SHAPE_REPRESENTATION('',(#5164),#8479);
#8601=SHAPE_REPRESENTATION('',(#5213),#8480);
#8602=SHAPE_REPRESENTATION('',(#5263),#8481);
#8603=SHAPE_REPRESENTATION('',(#5284),#8482);
#8604=SHAPE_REPRESENTATION('',(#5308),#8483);
#8605=SHAPE_REPRESENTATION('',(#5351),#8484);
#8606=SHAPE_REPRESENTATION('',(#5377),#8485);
#8607=SHAPE_REPRESENTATION('',(#5398),#8486);
#8608=SHAPE_REPRESENTATION('',(#5405),#8487);
#8609=SHAPE_REPRESENTATION('',(#5412,#5616,#5617,#5618,#5619,#5620,#5621,
#5622,#5623,#5624,#5625,#5626,#5627,#5628),#8488);
#8610=SHAPE_REPRESENTATION('',(#5413,#5475,#5476,#5477),#8489);
#8611=SHAPE_REPRESENTATION('',(#5414),#8490);
#8612=SHAPE_REPRESENTATION('',(#5453),#8491);
#8613=SHAPE_REPRESENTATION('',(#5464),#8492);
#8614=SHAPE_REPRESENTATION('',(#5478),#8493);
#8615=SHAPE_REPRESENTATION('',(#5503),#8494);
#8616=SHAPE_REPRESENTATION('',(#5512),#8495);
#8617=SHAPE_REPRESENTATION('',(#5523),#8496);
#8618=SHAPE_REPRESENTATION('',(#5581),#8497);
#8619=SHAPE_REPRESENTATION('',(#5590),#8498);
#8620=PRODUCT_DEFINITION_CONTEXT('part definition',#8688,'design');
#8621=PRODUCT_DEFINITION('PAT-074','PAT-074',
#8643,#8620);
#8622=PRODUCT_DEFINITION('Rail frame and stops','Rail frame and stops',
#8644,#8620);
#8623=PRODUCT_DEFINITION('Base plate','Base plate',#8645,#8620);
#8624=PRODUCT_DEFINITION('Slotted Extrusion - 20 x 20 x 300 mm',
'Slotted Extrusion - 20 x 20 x 300 mm',#8646,#8620);
#8625=PRODUCT_DEFINITION('Captive slot nut','Captive slot nut',#8647,#8620);
#8626=PRODUCT_DEFINITION('M5x14 Cap Screw','M5x14 Cap Screw',#8648,#8620);
#8627=PRODUCT_DEFINITION('Linear Guide Rail - 15 mm, 220 mm Long',
'Linear Guide Rail - 15 mm, 220 mm Long',#8649,#8620);
#8628=PRODUCT_DEFINITION('Cap Screw - M4x16','Cap Screw - M4x16',#8650,
#8620);
#8629=PRODUCT_DEFINITION('End stop','End stop',#8651,#8620);
#8630=PRODUCT_DEFINITION('Bonded stop pad','Bonded stop pad',#8652,#8620);
#8631=PRODUCT_DEFINITION('Bonded foot pad','Bonded foot pad',#8653,#8620);
#8632=PRODUCT_DEFINITION('Carriage table and grip',
'Carriage table and grip',#8654,#8620);
#8633=PRODUCT_DEFINITION('Flanged Linear Guide Carriage - 15 mm',
'Flanged Linear Guide Carriage - 15 mm',#8655,#8620);
#8634=PRODUCT_DEFINITION('Block','Block',#8656,#8620);
#8635=PRODUCT_DEFINITION('End cap +','End cap +',#8657,#8620);
#8636=PRODUCT_DEFINITION('End cap','End cap',#8658,#8620);
#8637=PRODUCT_DEFINITION('Table plate','Table plate',#8659,#8620);
#8638=PRODUCT_DEFINITION('Manual grip','Manual grip',#8660,#8620);
#8639=PRODUCT_DEFINITION('Flat Washer - M5','Flat Washer - M5',#8661,#8620);
#8640=PRODUCT_DEFINITION('Cap Screw - M5x20','Cap Screw - M5x20',#8662,
#8620);
#8641=PRODUCT_DEFINITION('Flat Washer - M6','Flat Washer - M6',#8663,#8620);
#8642=PRODUCT_DEFINITION('Cap Screw - M6x25','Cap Screw - M6x25',#8664,
#8620);
#8643=PRODUCT_DEFINITION_FORMATION('',$,#8690);
#8644=PRODUCT_DEFINITION_FORMATION('',$,#8691);
#8645=PRODUCT_DEFINITION_FORMATION('',$,#8692);
#8646=PRODUCT_DEFINITION_FORMATION('',$,#8693);
#8647=PRODUCT_DEFINITION_FORMATION('',$,#8694);
#8648=PRODUCT_DEFINITION_FORMATION('',$,#8695);
#8649=PRODUCT_DEFINITION_FORMATION('',$,#8696);
#8650=PRODUCT_DEFINITION_FORMATION('',$,#8697);
#8651=PRODUCT_DEFINITION_FORMATION('',$,#8698);
#8652=PRODUCT_DEFINITION_FORMATION('',$,#8699);
#8653=PRODUCT_DEFINITION_FORMATION('',$,#8700);
#8654=PRODUCT_DEFINITION_FORMATION('',$,#8701);
#8655=PRODUCT_DEFINITION_FORMATION('',$,#8702);
#8656=PRODUCT_DEFINITION_FORMATION('',$,#8703);
#8657=PRODUCT_DEFINITION_FORMATION('',$,#8704);
#8658=PRODUCT_DEFINITION_FORMATION('',$,#8705);
#8659=PRODUCT_DEFINITION_FORMATION('',$,#8706);
#8660=PRODUCT_DEFINITION_FORMATION('',$,#8707);
#8661=PRODUCT_DEFINITION_FORMATION('',$,#8708);
#8662=PRODUCT_DEFINITION_FORMATION('',$,#8709);
#8663=PRODUCT_DEFINITION_FORMATION('',$,#8710);
#8664=PRODUCT_DEFINITION_FORMATION('',$,#8711);
#8665=PRODUCT_RELATED_PRODUCT_CATEGORY('PAT-074','PAT-074',(#8690));
#8666=PRODUCT_RELATED_PRODUCT_CATEGORY('Rail frame and stops',
'Rail frame and stops',(#8691));
#8667=PRODUCT_RELATED_PRODUCT_CATEGORY('Base plate','Base plate',(#8692));
#8668=PRODUCT_RELATED_PRODUCT_CATEGORY(
'Slotted Extrusion - 20 x 20 x 300 mm',
'Slotted Extrusion - 20 x 20 x 300 mm',(#8693));
#8669=PRODUCT_RELATED_PRODUCT_CATEGORY('Captive slot nut',
'Captive slot nut',(#8694));
#8670=PRODUCT_RELATED_PRODUCT_CATEGORY('M5x14 Cap Screw',
'M5x14 Cap Screw',(#8695));
#8671=PRODUCT_RELATED_PRODUCT_CATEGORY(
'Linear Guide Rail - 15 mm, 220 mm Long',
'Linear Guide Rail - 15 mm, 220 mm Long',(#8696));
#8672=PRODUCT_RELATED_PRODUCT_CATEGORY('Cap Screw - M4x16',
'Cap Screw - M4x16',(#8697));
#8673=PRODUCT_RELATED_PRODUCT_CATEGORY('End stop','End stop',(#8698));
#8674=PRODUCT_RELATED_PRODUCT_CATEGORY('Bonded stop pad',
'Bonded stop pad',(#8699));
#8675=PRODUCT_RELATED_PRODUCT_CATEGORY('Bonded foot pad',
'Bonded foot pad',(#8700));
#8676=PRODUCT_RELATED_PRODUCT_CATEGORY('Carriage table and grip',
'Carriage table and grip',(#8701));
#8677=PRODUCT_RELATED_PRODUCT_CATEGORY(
'Flanged Linear Guide Carriage - 15 mm',
'Flanged Linear Guide Carriage - 15 mm',(#8702));
#8678=PRODUCT_RELATED_PRODUCT_CATEGORY('Block','Block',(#8703));
#8679=PRODUCT_RELATED_PRODUCT_CATEGORY('End cap +','End cap +',(#8704));
#8680=PRODUCT_RELATED_PRODUCT_CATEGORY('End cap','End cap',(#8705));
#8681=PRODUCT_RELATED_PRODUCT_CATEGORY('Table plate','Table plate',(#8706));
#8682=PRODUCT_RELATED_PRODUCT_CATEGORY('Manual grip','Manual grip',(#8707));
#8683=PRODUCT_RELATED_PRODUCT_CATEGORY('Flat Washer - M5',
'Flat Washer - M5',(#8708));
#8684=PRODUCT_RELATED_PRODUCT_CATEGORY('Cap Screw - M5x20',
'Cap Screw - M5x20',(#8709));
#8685=PRODUCT_RELATED_PRODUCT_CATEGORY('Flat Washer - M6',
'Flat Washer - M6',(#8710));
#8686=PRODUCT_RELATED_PRODUCT_CATEGORY('Cap Screw - M6x25',
'Cap Screw - M6x25',(#8711));
#8687=APPLICATION_PROTOCOL_DEFINITION('international standard',
'automotive_design',2009,#8688);
#8688=APPLICATION_CONTEXT(
'Core Data for Automotive Mechanical Design Process');
#8689=PRODUCT_CONTEXT('part definition',#8688,'mechanical');
#8690=PRODUCT('PAT-074','PAT-074',
'PAT-074',(#8689));
#8691=PRODUCT('Rail frame and stops','Rail frame and stops',
'Rail frame and stops',(#8689));
#8692=PRODUCT('Base plate','Base plate','Base plate',(#8689));
#8693=PRODUCT('Slotted Extrusion - 20 x 20 x 300 mm',
'Slotted Extrusion - 20 x 20 x 300 mm',
'Slotted Extrusion - 20 x 20 x 300 mm',(#8689));
#8694=PRODUCT('Captive slot nut','Captive slot nut','Captive slot nut',
(#8689));
#8695=PRODUCT('M5x14 Cap Screw','M5x14 Cap Screw','M5x14 Cap Screw',(#8689));
#8696=PRODUCT('Linear Guide Rail - 15 mm, 220 mm Long',
'Linear Guide Rail - 15 mm, 220 mm Long',
'Linear Guide Rail - 15 mm, 220 mm Long',(#8689));
#8697=PRODUCT('Cap Screw - M4x16','Cap Screw - M4x16',
'Cap Screw - M4x16',(#8689));
#8698=PRODUCT('End stop','End stop','End stop',(#8689));
#8699=PRODUCT('Bonded stop pad','Bonded stop pad','Bonded stop pad',(#8689));
#8700=PRODUCT('Bonded foot pad','Bonded foot pad','Bonded foot pad',(#8689));
#8701=PRODUCT('Carriage table and grip','Carriage table and grip',
'Carriage table and grip',(#8689));
#8702=PRODUCT('Flanged Linear Guide Carriage - 15 mm',
'Flanged Linear Guide Carriage - 15 mm',
'Flanged Linear Guide Carriage - 15 mm',(#8689));
#8703=PRODUCT('Block','Block','Block',(#8689));
#8704=PRODUCT('End cap +','End cap +','End cap +',(#8689));
#8705=PRODUCT('End cap','End cap','End cap',(#8689));
#8706=PRODUCT('Table plate','Table plate','Table plate',(#8689));
#8707=PRODUCT('Manual grip','Manual grip','Manual grip',(#8689));
#8708=PRODUCT('Flat Washer - M5','Flat Washer - M5','Flat Washer - M5',
(#8689));
#8709=PRODUCT('Cap Screw - M5x20','Cap Screw - M5x20',
'Cap Screw - M5x20',(#8689));
#8710=PRODUCT('Flat Washer - M6','Flat Washer - M6','Flat Washer - M6',
(#8689));
#8711=PRODUCT('Cap Screw - M6x25','Cap Screw - M6x25',
'Cap Screw - M6x25',(#8689));
#8712=PRESENTATION_STYLE_ASSIGNMENT((#8719));
#8713=PRESENTATION_STYLE_ASSIGNMENT((#8720));
#8714=PRESENTATION_STYLE_ASSIGNMENT((#8721));
#8715=PRESENTATION_STYLE_ASSIGNMENT((#8722));
#8716=PRESENTATION_STYLE_ASSIGNMENT((#8723));
#8717=PRESENTATION_STYLE_ASSIGNMENT((#8724));
#8718=PRESENTATION_STYLE_ASSIGNMENT((#8725));
#8719=SURFACE_STYLE_USAGE(.BOTH.,#8726);
#8720=SURFACE_STYLE_USAGE(.BOTH.,#8727);
#8721=SURFACE_STYLE_USAGE(.BOTH.,#8728);
#8722=SURFACE_STYLE_USAGE(.BOTH.,#8729);
#8723=SURFACE_STYLE_USAGE(.BOTH.,#8730);
#8724=SURFACE_STYLE_USAGE(.BOTH.,#8731);
#8725=SURFACE_STYLE_USAGE(.BOTH.,#8732);
#8726=SURFACE_SIDE_STYLE('',(#8733));
#8727=SURFACE_SIDE_STYLE('',(#8734));
#8728=SURFACE_SIDE_STYLE('',(#8735));
#8729=SURFACE_SIDE_STYLE('',(#8736));
#8730=SURFACE_SIDE_STYLE('',(#8737));
#8731=SURFACE_SIDE_STYLE('',(#8738));
#8732=SURFACE_SIDE_STYLE('',(#8739));
#8733=SURFACE_STYLE_FILL_AREA(#8740);
#8734=SURFACE_STYLE_FILL_AREA(#8741);
#8735=SURFACE_STYLE_FILL_AREA(#8742);
#8736=SURFACE_STYLE_FILL_AREA(#8743);
#8737=SURFACE_STYLE_FILL_AREA(#8744);
#8738=SURFACE_STYLE_FILL_AREA(#8745);
#8739=SURFACE_STYLE_FILL_AREA(#8746);
#8740=FILL_AREA_STYLE('Steel - Satin',(#8747));
#8741=FILL_AREA_STYLE('CAD Library Painted - Deep blue',(#8748));
#8742=FILL_AREA_STYLE('CAD Library Painted - Steel gray',(#8749));
#8743=FILL_AREA_STYLE('CAD Library Painted - Engineering blue',(#8750));
#8744=FILL_AREA_STYLE('CAD Library Painted - Graphite',(#8751));
#8745=FILL_AREA_STYLE('CAD Library Painted - Off white',(#8752));
#8746=FILL_AREA_STYLE('CAD Library Painted - Light blue',(#8753));
#8747=FILL_AREA_STYLE_COLOUR('Steel - Satin',#8754);
#8748=FILL_AREA_STYLE_COLOUR('CAD Library Painted - Deep blue',#8755);
#8749=FILL_AREA_STYLE_COLOUR('CAD Library Painted - Steel gray',#8756);
#8750=FILL_AREA_STYLE_COLOUR('CAD Library Painted - Engineering blue',#8757);
#8751=FILL_AREA_STYLE_COLOUR('CAD Library Painted - Graphite',#8758);
#8752=FILL_AREA_STYLE_COLOUR('CAD Library Painted - Off white',#8759);
#8753=FILL_AREA_STYLE_COLOUR('CAD Library Painted - Light blue',#8760);
#8754=COLOUR_RGB('Steel - Satin',0.627450980392157,0.627450980392157,0.627450980392157);
#8755=COLOUR_RGB('CAD Library Painted - Deep blue',0.0784313725490196,0.203921568627451,
0.349019607843137);
#8756=COLOUR_RGB('CAD Library Painted - Steel gray',0.592156862745098,0.631372549019608,
0.67843137254902);
#8757=COLOUR_RGB('CAD Library Painted - Engineering blue',0.12156862745098,
0.356862745098039,0.6);
#8758=COLOUR_RGB('CAD Library Painted - Graphite',0.0980392156862745,0.109803921568627,
0.125490196078431);
#8759=COLOUR_RGB('CAD Library Painted - Off white',0.909803921568627,0.901960784313726,
0.858823529411765);
#8760=COLOUR_RGB('CAD Library Painted - Light blue',0.286274509803922,0.552941176470588,
0.780392156862745);
#8761=COLOUR_RGB('Dark Blue',0.08,0.2,0.34);
#8762=FILL_AREA_STYLE_COLOUR('',#8761);
#8763=FILL_AREA_STYLE('',(#8762));
#8764=SURFACE_STYLE_FILL_AREA(#8763);
#8765=SURFACE_SIDE_STYLE('',(#8764));
#8766=SURFACE_STYLE_USAGE(.BOTH.,#8765);
#8767=PRESENTATION_STYLE_ASSIGNMENT((#8766));
#8768=COLOUR_RGB('Light Blue',0.38,0.62,0.78);
#8769=FILL_AREA_STYLE_COLOUR('',#8768);
#8770=FILL_AREA_STYLE('',(#8769));
#8771=SURFACE_STYLE_FILL_AREA(#8770);
#8772=SURFACE_SIDE_STYLE('',(#8771));
#8773=SURFACE_STYLE_USAGE(.BOTH.,#8772);
#8774=PRESENTATION_STYLE_ASSIGNMENT((#8773));
#8775=COLOUR_RGB('Sky Blue',0.24,0.69,0.87);
#8776=FILL_AREA_STYLE_COLOUR('',#8775);
#8777=FILL_AREA_STYLE('',(#8776));
#8778=SURFACE_STYLE_FILL_AREA(#8777);
#8779=SURFACE_SIDE_STYLE('',(#8778));
#8780=SURFACE_STYLE_USAGE(.BOTH.,#8779);
#8781=PRESENTATION_STYLE_ASSIGNMENT((#8780));
#8782=COLOUR_RGB('Grey',0.48,0.52,0.57);
#8783=FILL_AREA_STYLE_COLOUR('',#8782);
#8784=FILL_AREA_STYLE('',(#8783));
#8785=SURFACE_STYLE_FILL_AREA(#8784);
#8786=SURFACE_SIDE_STYLE('',(#8785));
#8787=SURFACE_STYLE_USAGE(.BOTH.,#8786);
#8788=PRESENTATION_STYLE_ASSIGNMENT((#8787));
#8789=COLOUR_RGB('Black',0.12,0.14,0.17);
#8790=FILL_AREA_STYLE_COLOUR('',#8789);
#8791=FILL_AREA_STYLE('',(#8790));
#8792=SURFACE_STYLE_FILL_AREA(#8791);
#8793=SURFACE_SIDE_STYLE('',(#8792));
#8794=SURFACE_STYLE_USAGE(.BOTH.,#8793);
#8795=PRESENTATION_STYLE_ASSIGNMENT((#8794));
#8796=COLOUR_RGB('Off White',0.89,0.88,0.83);
#8797=FILL_AREA_STYLE_COLOUR('',#8796);
#8798=FILL_AREA_STYLE('',(#8797));
#8799=SURFACE_STYLE_FILL_AREA(#8798);
#8800=SURFACE_SIDE_STYLE('',(#8799));
#8801=SURFACE_STYLE_USAGE(.BOTH.,#8800);
#8802=PRESENTATION_STYLE_ASSIGNMENT((#8801));
ENDSEC;
END-ISO-10303-21;
